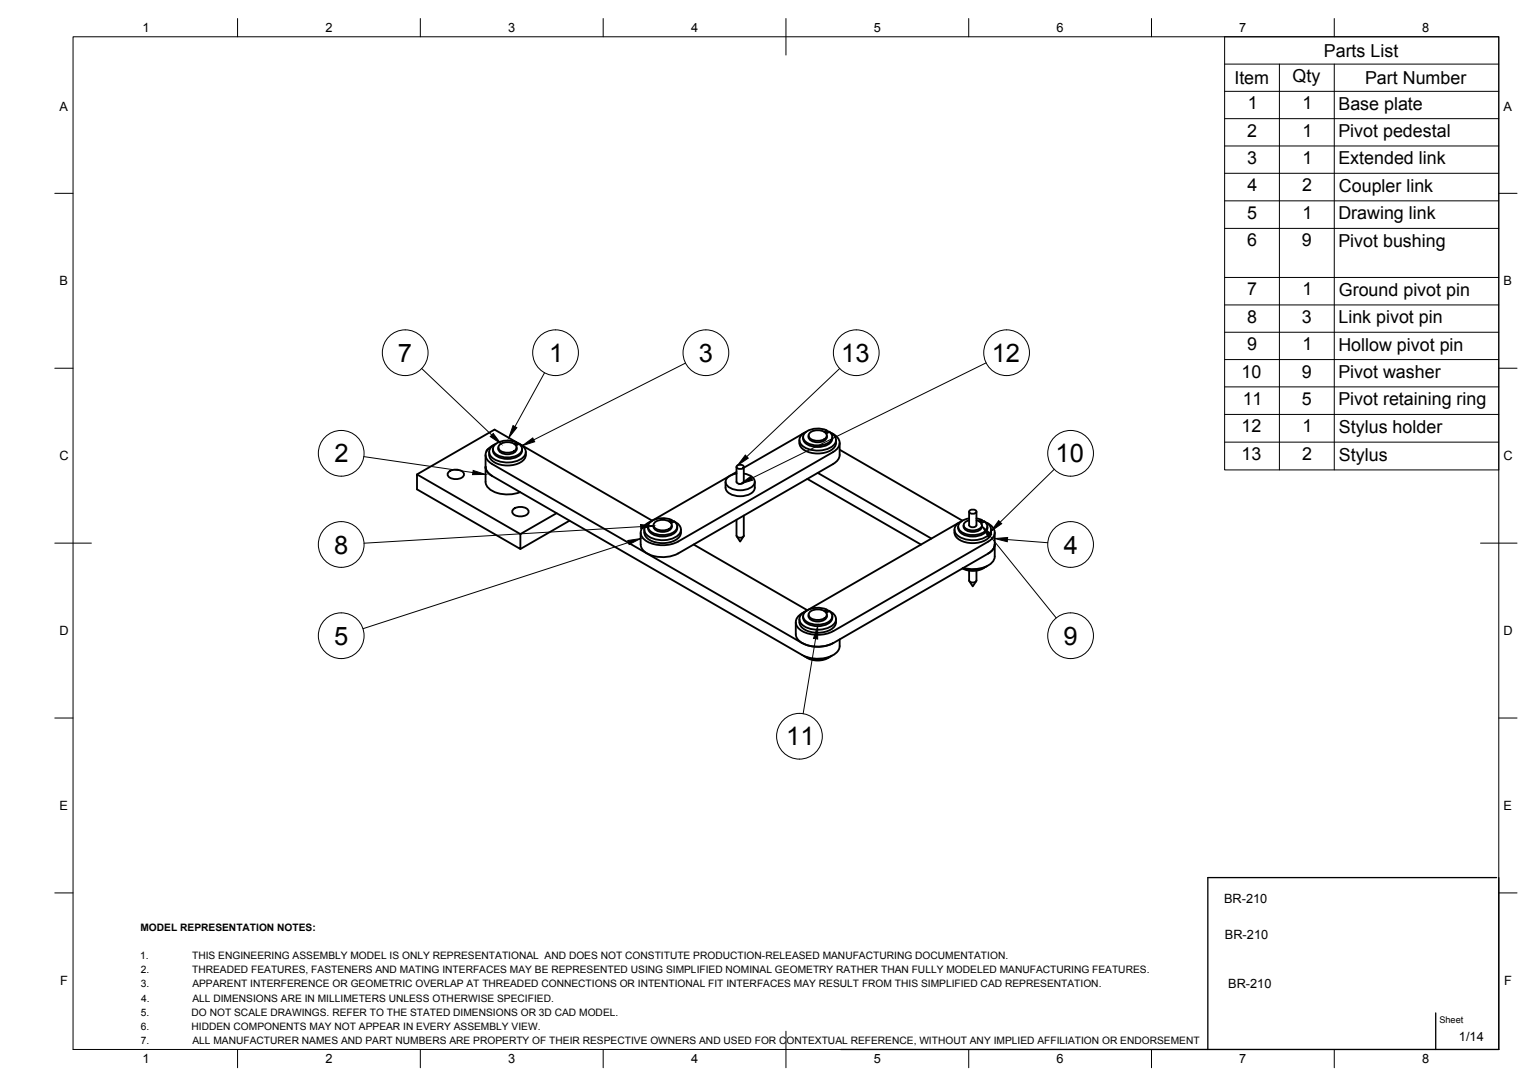
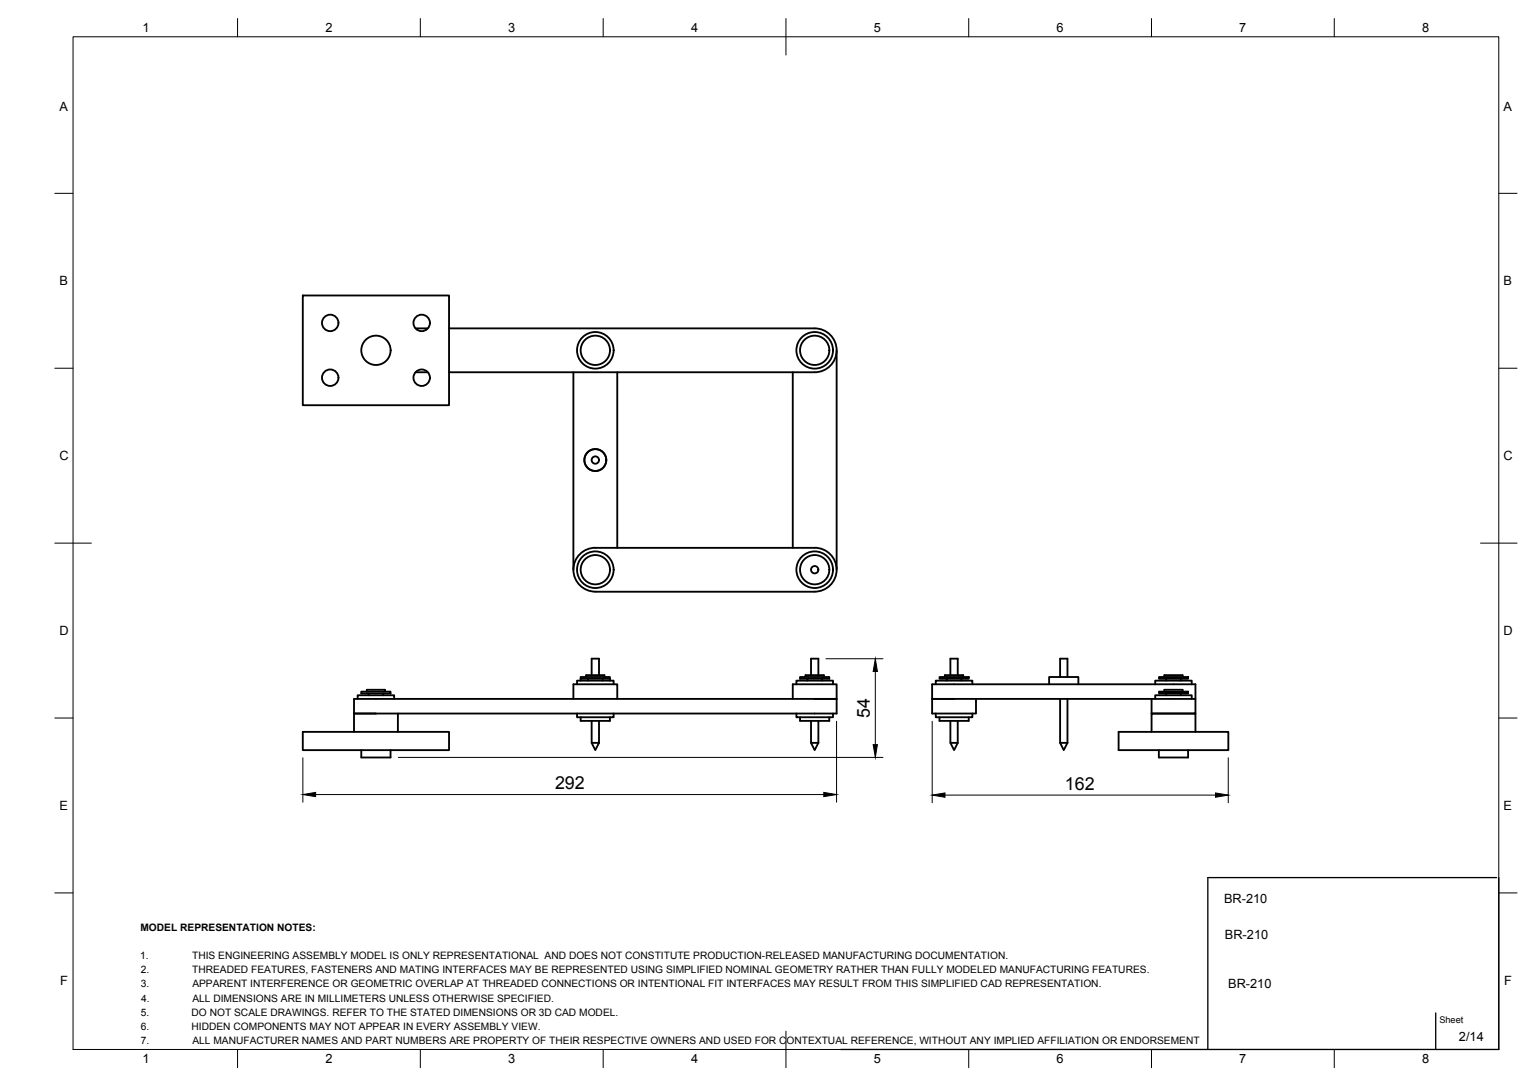
ISO-10303-21;
HEADER;
/* Generated by software containing ST-Developer
 * from STEP Tools, Inc. (www.steptools.com) 
 */

FILE_DESCRIPTION(
/* description */ ('Independent 1:2 reduction pantograph. 120 mm parallelogram sides; fix
ed fulcrum on the extension of a 240 mm link. Drawing point halfway al
ong its link, so its XY displacement is one half of the tracing point.
 Replaceable pivot bushes and retained pins. Calibration and productio
n accuracy unassigned.'),
/* implementation_level */ '2;1');

FILE_NAME(
/* name */ 'BR-210.step',
/* time_stamp */ '2026-11-07T22:11:57-08:00',
/* author */ (''),
/* organization */ (''),
/* preprocessor_version */ 'ST-DEVELOPER v20.2',
/* originating_system */ 'Autodesk Translation Framework v15.17.0.0',
/* authorisation */ '');

FILE_SCHEMA (('AUTOMOTIVE_DESIGN { 1 0 10303 214 3 1 1 }'));
ENDSEC;

DATA;
#10=MECHANICAL_DESIGN_GEOMETRIC_PRESENTATION_REPRESENTATION('',(#186,#187,
#188,#189,#190,#191,#192,#193,#194,#195,#196,#197,#198),#2926);
#11=ITEM_DEFINED_TRANSFORMATION($,$,#1699,#1892);
#12=ITEM_DEFINED_TRANSFORMATION($,$,#1721,#1893);
#13=ITEM_DEFINED_TRANSFORMATION($,$,#1730,#1894);
#14=ITEM_DEFINED_TRANSFORMATION($,$,#1822,#1895);
#15=ITEM_DEFINED_TRANSFORMATION($,$,#1750,#1896);
#16=ITEM_DEFINED_TRANSFORMATION($,$,#1839,#1897);
#17=ITEM_DEFINED_TRANSFORMATION($,$,#1770,#1898);
#18=ITEM_DEFINED_TRANSFORMATION($,$,#1848,#1899);
#19=ITEM_DEFINED_TRANSFORMATION($,$,#1788,#1900);
#20=ITEM_DEFINED_TRANSFORMATION($,$,#1866,#1901);
#21=ITEM_DEFINED_TRANSFORMATION($,$,#1875,#1902);
#22=ITEM_DEFINED_TRANSFORMATION($,$,#1809,#1903);
#23=ITEM_DEFINED_TRANSFORMATION($,$,#1886,#1904);
#24=ITEM_DEFINED_TRANSFORMATION($,$,#1822,#1905);
#25=ITEM_DEFINED_TRANSFORMATION($,$,#1839,#1906);
#26=ITEM_DEFINED_TRANSFORMATION($,$,#1839,#1907);
#27=ITEM_DEFINED_TRANSFORMATION($,$,#1839,#1908);
#28=ITEM_DEFINED_TRANSFORMATION($,$,#1839,#1909);
#29=ITEM_DEFINED_TRANSFORMATION($,$,#1839,#1910);
#30=ITEM_DEFINED_TRANSFORMATION($,$,#1839,#1911);
#31=ITEM_DEFINED_TRANSFORMATION($,$,#1839,#1912);
#32=ITEM_DEFINED_TRANSFORMATION($,$,#1839,#1913);
#33=ITEM_DEFINED_TRANSFORMATION($,$,#1866,#1914);
#34=ITEM_DEFINED_TRANSFORMATION($,$,#1866,#1915);
#35=ITEM_DEFINED_TRANSFORMATION($,$,#1875,#1916);
#36=ITEM_DEFINED_TRANSFORMATION($,$,#1848,#1917);
#37=ITEM_DEFINED_TRANSFORMATION($,$,#1866,#1918);
#38=ITEM_DEFINED_TRANSFORMATION($,$,#1866,#1919);
#39=ITEM_DEFINED_TRANSFORMATION($,$,#1875,#1920);
#40=ITEM_DEFINED_TRANSFORMATION($,$,#1848,#1921);
#41=ITEM_DEFINED_TRANSFORMATION($,$,#1866,#1922);
#42=ITEM_DEFINED_TRANSFORMATION($,$,#1866,#1923);
#43=ITEM_DEFINED_TRANSFORMATION($,$,#1875,#1924);
#44=ITEM_DEFINED_TRANSFORMATION($,$,#1866,#1925);
#45=ITEM_DEFINED_TRANSFORMATION($,$,#1866,#1926);
#46=ITEM_DEFINED_TRANSFORMATION($,$,#1875,#1927);
#47=ITEM_DEFINED_TRANSFORMATION($,$,#1886,#1928);
#48=(
REPRESENTATION_RELATIONSHIP($,$,#2997,#2996)
REPRESENTATION_RELATIONSHIP_WITH_TRANSFORMATION(#11)
SHAPE_REPRESENTATION_RELATIONSHIP()
);
#49=(
REPRESENTATION_RELATIONSHIP($,$,#2998,#2996)
REPRESENTATION_RELATIONSHIP_WITH_TRANSFORMATION(#12)
SHAPE_REPRESENTATION_RELATIONSHIP()
);
#50=(
REPRESENTATION_RELATIONSHIP($,$,#2999,#2996)
REPRESENTATION_RELATIONSHIP_WITH_TRANSFORMATION(#13)
SHAPE_REPRESENTATION_RELATIONSHIP()
);
#51=(
REPRESENTATION_RELATIONSHIP($,$,#3004,#2996)
REPRESENTATION_RELATIONSHIP_WITH_TRANSFORMATION(#14)
SHAPE_REPRESENTATION_RELATIONSHIP()
);
#52=(
REPRESENTATION_RELATIONSHIP($,$,#3000,#2996)
REPRESENTATION_RELATIONSHIP_WITH_TRANSFORMATION(#15)
SHAPE_REPRESENTATION_RELATIONSHIP()
);
#53=(
REPRESENTATION_RELATIONSHIP($,$,#3005,#2996)
REPRESENTATION_RELATIONSHIP_WITH_TRANSFORMATION(#16)
SHAPE_REPRESENTATION_RELATIONSHIP()
);
#54=(
REPRESENTATION_RELATIONSHIP($,$,#3001,#2996)
REPRESENTATION_RELATIONSHIP_WITH_TRANSFORMATION(#17)
SHAPE_REPRESENTATION_RELATIONSHIP()
);
#55=(
REPRESENTATION_RELATIONSHIP($,$,#3006,#2996)
REPRESENTATION_RELATIONSHIP_WITH_TRANSFORMATION(#18)
SHAPE_REPRESENTATION_RELATIONSHIP()
);
#56=(
REPRESENTATION_RELATIONSHIP($,$,#3002,#2996)
REPRESENTATION_RELATIONSHIP_WITH_TRANSFORMATION(#19)
SHAPE_REPRESENTATION_RELATIONSHIP()
);
#57=(
REPRESENTATION_RELATIONSHIP($,$,#3007,#2996)
REPRESENTATION_RELATIONSHIP_WITH_TRANSFORMATION(#20)
SHAPE_REPRESENTATION_RELATIONSHIP()
);
#58=(
REPRESENTATION_RELATIONSHIP($,$,#3008,#2996)
REPRESENTATION_RELATIONSHIP_WITH_TRANSFORMATION(#21)
SHAPE_REPRESENTATION_RELATIONSHIP()
);
#59=(
REPRESENTATION_RELATIONSHIP($,$,#3003,#2996)
REPRESENTATION_RELATIONSHIP_WITH_TRANSFORMATION(#22)
SHAPE_REPRESENTATION_RELATIONSHIP()
);
#60=(
REPRESENTATION_RELATIONSHIP($,$,#3009,#2996)
REPRESENTATION_RELATIONSHIP_WITH_TRANSFORMATION(#23)
SHAPE_REPRESENTATION_RELATIONSHIP()
);
#61=(
REPRESENTATION_RELATIONSHIP($,$,#3004,#2996)
REPRESENTATION_RELATIONSHIP_WITH_TRANSFORMATION(#24)
SHAPE_REPRESENTATION_RELATIONSHIP()
);
#62=(
REPRESENTATION_RELATIONSHIP($,$,#3005,#2996)
REPRESENTATION_RELATIONSHIP_WITH_TRANSFORMATION(#25)
SHAPE_REPRESENTATION_RELATIONSHIP()
);
#63=(
REPRESENTATION_RELATIONSHIP($,$,#3005,#2996)
REPRESENTATION_RELATIONSHIP_WITH_TRANSFORMATION(#26)
SHAPE_REPRESENTATION_RELATIONSHIP()
);
#64=(
REPRESENTATION_RELATIONSHIP($,$,#3005,#2996)
REPRESENTATION_RELATIONSHIP_WITH_TRANSFORMATION(#27)
SHAPE_REPRESENTATION_RELATIONSHIP()
);
#65=(
REPRESENTATION_RELATIONSHIP($,$,#3005,#2996)
REPRESENTATION_RELATIONSHIP_WITH_TRANSFORMATION(#28)
SHAPE_REPRESENTATION_RELATIONSHIP()
);
#66=(
REPRESENTATION_RELATIONSHIP($,$,#3005,#2996)
REPRESENTATION_RELATIONSHIP_WITH_TRANSFORMATION(#29)
SHAPE_REPRESENTATION_RELATIONSHIP()
);
#67=(
REPRESENTATION_RELATIONSHIP($,$,#3005,#2996)
REPRESENTATION_RELATIONSHIP_WITH_TRANSFORMATION(#30)
SHAPE_REPRESENTATION_RELATIONSHIP()
);
#68=(
REPRESENTATION_RELATIONSHIP($,$,#3005,#2996)
REPRESENTATION_RELATIONSHIP_WITH_TRANSFORMATION(#31)
SHAPE_REPRESENTATION_RELATIONSHIP()
);
#69=(
REPRESENTATION_RELATIONSHIP($,$,#3005,#2996)
REPRESENTATION_RELATIONSHIP_WITH_TRANSFORMATION(#32)
SHAPE_REPRESENTATION_RELATIONSHIP()
);
#70=(
REPRESENTATION_RELATIONSHIP($,$,#3007,#2996)
REPRESENTATION_RELATIONSHIP_WITH_TRANSFORMATION(#33)
SHAPE_REPRESENTATION_RELATIONSHIP()
);
#71=(
REPRESENTATION_RELATIONSHIP($,$,#3007,#2996)
REPRESENTATION_RELATIONSHIP_WITH_TRANSFORMATION(#34)
SHAPE_REPRESENTATION_RELATIONSHIP()
);
#72=(
REPRESENTATION_RELATIONSHIP($,$,#3008,#2996)
REPRESENTATION_RELATIONSHIP_WITH_TRANSFORMATION(#35)
SHAPE_REPRESENTATION_RELATIONSHIP()
);
#73=(
REPRESENTATION_RELATIONSHIP($,$,#3006,#2996)
REPRESENTATION_RELATIONSHIP_WITH_TRANSFORMATION(#36)
SHAPE_REPRESENTATION_RELATIONSHIP()
);
#74=(
REPRESENTATION_RELATIONSHIP($,$,#3007,#2996)
REPRESENTATION_RELATIONSHIP_WITH_TRANSFORMATION(#37)
SHAPE_REPRESENTATION_RELATIONSHIP()
);
#75=(
REPRESENTATION_RELATIONSHIP($,$,#3007,#2996)
REPRESENTATION_RELATIONSHIP_WITH_TRANSFORMATION(#38)
SHAPE_REPRESENTATION_RELATIONSHIP()
);
#76=(
REPRESENTATION_RELATIONSHIP($,$,#3008,#2996)
REPRESENTATION_RELATIONSHIP_WITH_TRANSFORMATION(#39)
SHAPE_REPRESENTATION_RELATIONSHIP()
);
#77=(
REPRESENTATION_RELATIONSHIP($,$,#3006,#2996)
REPRESENTATION_RELATIONSHIP_WITH_TRANSFORMATION(#40)
SHAPE_REPRESENTATION_RELATIONSHIP()
);
#78=(
REPRESENTATION_RELATIONSHIP($,$,#3007,#2996)
REPRESENTATION_RELATIONSHIP_WITH_TRANSFORMATION(#41)
SHAPE_REPRESENTATION_RELATIONSHIP()
);
#79=(
REPRESENTATION_RELATIONSHIP($,$,#3007,#2996)
REPRESENTATION_RELATIONSHIP_WITH_TRANSFORMATION(#42)
SHAPE_REPRESENTATION_RELATIONSHIP()
);
#80=(
REPRESENTATION_RELATIONSHIP($,$,#3008,#2996)
REPRESENTATION_RELATIONSHIP_WITH_TRANSFORMATION(#43)
SHAPE_REPRESENTATION_RELATIONSHIP()
);
#81=(
REPRESENTATION_RELATIONSHIP($,$,#3007,#2996)
REPRESENTATION_RELATIONSHIP_WITH_TRANSFORMATION(#44)
SHAPE_REPRESENTATION_RELATIONSHIP()
);
#82=(
REPRESENTATION_RELATIONSHIP($,$,#3007,#2996)
REPRESENTATION_RELATIONSHIP_WITH_TRANSFORMATION(#45)
SHAPE_REPRESENTATION_RELATIONSHIP()
);
#83=(
REPRESENTATION_RELATIONSHIP($,$,#3008,#2996)
REPRESENTATION_RELATIONSHIP_WITH_TRANSFORMATION(#46)
SHAPE_REPRESENTATION_RELATIONSHIP()
);
#84=(
REPRESENTATION_RELATIONSHIP($,$,#3009,#2996)
REPRESENTATION_RELATIONSHIP_WITH_TRANSFORMATION(#47)
SHAPE_REPRESENTATION_RELATIONSHIP()
);
#85=CONTEXT_DEPENDENT_SHAPE_REPRESENTATION(#48,#2959);
#86=CONTEXT_DEPENDENT_SHAPE_REPRESENTATION(#49,#2960);
#87=CONTEXT_DEPENDENT_SHAPE_REPRESENTATION(#50,#2961);
#88=CONTEXT_DEPENDENT_SHAPE_REPRESENTATION(#51,#2962);
#89=CONTEXT_DEPENDENT_SHAPE_REPRESENTATION(#52,#2963);
#90=CONTEXT_DEPENDENT_SHAPE_REPRESENTATION(#53,#2964);
#91=CONTEXT_DEPENDENT_SHAPE_REPRESENTATION(#54,#2965);
#92=CONTEXT_DEPENDENT_SHAPE_REPRESENTATION(#55,#2966);
#93=CONTEXT_DEPENDENT_SHAPE_REPRESENTATION(#56,#2967);
#94=CONTEXT_DEPENDENT_SHAPE_REPRESENTATION(#57,#2968);
#95=CONTEXT_DEPENDENT_SHAPE_REPRESENTATION(#58,#2969);
#96=CONTEXT_DEPENDENT_SHAPE_REPRESENTATION(#59,#2970);
#97=CONTEXT_DEPENDENT_SHAPE_REPRESENTATION(#60,#2971);
#98=CONTEXT_DEPENDENT_SHAPE_REPRESENTATION(#61,#2972);
#99=CONTEXT_DEPENDENT_SHAPE_REPRESENTATION(#62,#2973);
#100=CONTEXT_DEPENDENT_SHAPE_REPRESENTATION(#63,#2974);
#101=CONTEXT_DEPENDENT_SHAPE_REPRESENTATION(#64,#2975);
#102=CONTEXT_DEPENDENT_SHAPE_REPRESENTATION(#65,#2976);
#103=CONTEXT_DEPENDENT_SHAPE_REPRESENTATION(#66,#2977);
#104=CONTEXT_DEPENDENT_SHAPE_REPRESENTATION(#67,#2978);
#105=CONTEXT_DEPENDENT_SHAPE_REPRESENTATION(#68,#2979);
#106=CONTEXT_DEPENDENT_SHAPE_REPRESENTATION(#69,#2980);
#107=CONTEXT_DEPENDENT_SHAPE_REPRESENTATION(#70,#2981);
#108=CONTEXT_DEPENDENT_SHAPE_REPRESENTATION(#71,#2982);
#109=CONTEXT_DEPENDENT_SHAPE_REPRESENTATION(#72,#2983);
#110=CONTEXT_DEPENDENT_SHAPE_REPRESENTATION(#73,#2984);
#111=CONTEXT_DEPENDENT_SHAPE_REPRESENTATION(#74,#2985);
#112=CONTEXT_DEPENDENT_SHAPE_REPRESENTATION(#75,#2986);
#113=CONTEXT_DEPENDENT_SHAPE_REPRESENTATION(#76,#2987);
#114=CONTEXT_DEPENDENT_SHAPE_REPRESENTATION(#77,#2988);
#115=CONTEXT_DEPENDENT_SHAPE_REPRESENTATION(#78,#2989);
#116=CONTEXT_DEPENDENT_SHAPE_REPRESENTATION(#79,#2990);
#117=CONTEXT_DEPENDENT_SHAPE_REPRESENTATION(#80,#2991);
#118=CONTEXT_DEPENDENT_SHAPE_REPRESENTATION(#81,#2992);
#119=CONTEXT_DEPENDENT_SHAPE_REPRESENTATION(#82,#2993);
#120=CONTEXT_DEPENDENT_SHAPE_REPRESENTATION(#83,#2994);
#121=CONTEXT_DEPENDENT_SHAPE_REPRESENTATION(#84,#2995);
#122=NEXT_ASSEMBLY_USAGE_OCCURRENCE('Base plate:1','Base plate:1',
'Base plate:1',#3011,#3012,'Base plate:1');
#123=NEXT_ASSEMBLY_USAGE_OCCURRENCE('Pivot pedestal:1',
'Pivot pedestal:1','Pivot pedestal:1',#3011,#3013,'Pivot pedestal:1');
#124=NEXT_ASSEMBLY_USAGE_OCCURRENCE('Extended link:1','Extended link:1',
'Extended link:1',#3011,#3014,'Extended link:1');
#125=NEXT_ASSEMBLY_USAGE_OCCURRENCE('Coupler link:1','Coupler link:1',
'Coupler link:1',#3011,#3019,'Coupler link:1');
#126=NEXT_ASSEMBLY_USAGE_OCCURRENCE('Drawing link:1','Drawing link:1',
'Drawing link:1',#3011,#3015,'Drawing link:1');
#127=NEXT_ASSEMBLY_USAGE_OCCURRENCE('Pivot bushing:1','Pivot bushing:1',
'Pivot bushing:1',#3011,#3020,'Pivot bushing:1');
#128=NEXT_ASSEMBLY_USAGE_OCCURRENCE('Ground pivot pin:1',
'Ground pivot pin:1','Ground pivot pin:1',#3011,#3016,
'Ground pivot pin:1');
#129=NEXT_ASSEMBLY_USAGE_OCCURRENCE('Link pivot pin:1',
'Link pivot pin:1','Link pivot pin:1',#3011,#3021,'Link pivot pin:1');
#130=NEXT_ASSEMBLY_USAGE_OCCURRENCE('Hollow pivot pin:1',
'Hollow pivot pin:1','Hollow pivot pin:1',#3011,#3017,
'Hollow pivot pin:1');
#131=NEXT_ASSEMBLY_USAGE_OCCURRENCE('Pivot washer:1','Pivot washer:1',
'Pivot washer:1',#3011,#3022,'Pivot washer:1');
#132=NEXT_ASSEMBLY_USAGE_OCCURRENCE('Pivot retaining ring:1',
'Pivot retaining ring:1','Pivot retaining ring:1',#3011,#3023,
'Pivot retaining ring:1');
#133=NEXT_ASSEMBLY_USAGE_OCCURRENCE('Stylus holder:1','Stylus holder:1',
'Stylus holder:1',#3011,#3018,'Stylus holder:1');
#134=NEXT_ASSEMBLY_USAGE_OCCURRENCE('Stylus:1','Stylus:1','Stylus:1',#3011,
#3024,'Stylus:1');
#135=NEXT_ASSEMBLY_USAGE_OCCURRENCE('Coupler link:2','Coupler link:2',
'Coupler link:2',#3011,#3019,'Coupler link:2');
#136=NEXT_ASSEMBLY_USAGE_OCCURRENCE('Pivot bushing:2','Pivot bushing:2',
'Pivot bushing:2',#3011,#3020,'Pivot bushing:2');
#137=NEXT_ASSEMBLY_USAGE_OCCURRENCE('Pivot bushing:3','Pivot bushing:3',
'Pivot bushing:3',#3011,#3020,'Pivot bushing:3');
#138=NEXT_ASSEMBLY_USAGE_OCCURRENCE('Pivot bushing:4','Pivot bushing:4',
'Pivot bushing:4',#3011,#3020,'Pivot bushing:4');
#139=NEXT_ASSEMBLY_USAGE_OCCURRENCE('Pivot bushing:5','Pivot bushing:5',
'Pivot bushing:5',#3011,#3020,'Pivot bushing:5');
#140=NEXT_ASSEMBLY_USAGE_OCCURRENCE('Pivot bushing:6','Pivot bushing:6',
'Pivot bushing:6',#3011,#3020,'Pivot bushing:6');
#141=NEXT_ASSEMBLY_USAGE_OCCURRENCE('Pivot bushing:7','Pivot bushing:7',
'Pivot bushing:7',#3011,#3020,'Pivot bushing:7');
#142=NEXT_ASSEMBLY_USAGE_OCCURRENCE('Pivot bushing:8','Pivot bushing:8',
'Pivot bushing:8',#3011,#3020,'Pivot bushing:8');
#143=NEXT_ASSEMBLY_USAGE_OCCURRENCE('Pivot bushing:9','Pivot bushing:9',
'Pivot bushing:9',#3011,#3020,'Pivot bushing:9');
#144=NEXT_ASSEMBLY_USAGE_OCCURRENCE('Pivot washer:2','Pivot washer:2',
'Pivot washer:2',#3011,#3022,'Pivot washer:2');
#145=NEXT_ASSEMBLY_USAGE_OCCURRENCE('Pivot washer:3','Pivot washer:3',
'Pivot washer:3',#3011,#3022,'Pivot washer:3');
#146=NEXT_ASSEMBLY_USAGE_OCCURRENCE('Pivot retaining ring:2',
'Pivot retaining ring:2','Pivot retaining ring:2',#3011,#3023,
'Pivot retaining ring:2');
#147=NEXT_ASSEMBLY_USAGE_OCCURRENCE('Link pivot pin:2',
'Link pivot pin:2','Link pivot pin:2',#3011,#3021,'Link pivot pin:2');
#148=NEXT_ASSEMBLY_USAGE_OCCURRENCE('Pivot washer:4','Pivot washer:4',
'Pivot washer:4',#3011,#3022,'Pivot washer:4');
#149=NEXT_ASSEMBLY_USAGE_OCCURRENCE('Pivot washer:5','Pivot washer:5',
'Pivot washer:5',#3011,#3022,'Pivot washer:5');
#150=NEXT_ASSEMBLY_USAGE_OCCURRENCE('Pivot retaining ring:3',
'Pivot retaining ring:3','Pivot retaining ring:3',#3011,#3023,
'Pivot retaining ring:3');
#151=NEXT_ASSEMBLY_USAGE_OCCURRENCE('Link pivot pin:3',
'Link pivot pin:3','Link pivot pin:3',#3011,#3021,'Link pivot pin:3');
#152=NEXT_ASSEMBLY_USAGE_OCCURRENCE('Pivot washer:6','Pivot washer:6',
'Pivot washer:6',#3011,#3022,'Pivot washer:6');
#153=NEXT_ASSEMBLY_USAGE_OCCURRENCE('Pivot washer:7','Pivot washer:7',
'Pivot washer:7',#3011,#3022,'Pivot washer:7');
#154=NEXT_ASSEMBLY_USAGE_OCCURRENCE('Pivot retaining ring:4',
'Pivot retaining ring:4','Pivot retaining ring:4',#3011,#3023,
'Pivot retaining ring:4');
#155=NEXT_ASSEMBLY_USAGE_OCCURRENCE('Pivot washer:8','Pivot washer:8',
'Pivot washer:8',#3011,#3022,'Pivot washer:8');
#156=NEXT_ASSEMBLY_USAGE_OCCURRENCE('Pivot washer:9','Pivot washer:9',
'Pivot washer:9',#3011,#3022,'Pivot washer:9');
#157=NEXT_ASSEMBLY_USAGE_OCCURRENCE('Pivot retaining ring:5',
'Pivot retaining ring:5','Pivot retaining ring:5',#3011,#3023,
'Pivot retaining ring:5');
#158=NEXT_ASSEMBLY_USAGE_OCCURRENCE('Stylus:2','Stylus:2','Stylus:2',#3011,
#3024,'Stylus:2');
#159=CONICAL_SURFACE('',#1891,1.,0.463647609000806);
#160=SHAPE_REPRESENTATION_RELATIONSHIP('SRR','None',#2997,#173);
#161=SHAPE_REPRESENTATION_RELATIONSHIP('SRR','None',#2998,#174);
#162=SHAPE_REPRESENTATION_RELATIONSHIP('SRR','None',#2999,#175);
#163=SHAPE_REPRESENTATION_RELATIONSHIP('SRR','None',#3000,#176);
#164=SHAPE_REPRESENTATION_RELATIONSHIP('SRR','None',#3001,#177);
#165=SHAPE_REPRESENTATION_RELATIONSHIP('SRR','None',#3002,#178);
#166=SHAPE_REPRESENTATION_RELATIONSHIP('SRR','None',#3003,#179);
#167=SHAPE_REPRESENTATION_RELATIONSHIP('SRR','None',#3004,#180);
#168=SHAPE_REPRESENTATION_RELATIONSHIP('SRR','None',#3005,#181);
#169=SHAPE_REPRESENTATION_RELATIONSHIP('SRR','None',#3006,#182);
#170=SHAPE_REPRESENTATION_RELATIONSHIP('SRR','None',#3007,#183);
#171=SHAPE_REPRESENTATION_RELATIONSHIP('SRR','None',#3008,#184);
#172=SHAPE_REPRESENTATION_RELATIONSHIP('SRR','None',#3009,#185);
#173=ADVANCED_BREP_SHAPE_REPRESENTATION('',(#199),#2913);
#174=ADVANCED_BREP_SHAPE_REPRESENTATION('',(#200),#2914);
#175=ADVANCED_BREP_SHAPE_REPRESENTATION('',(#201),#2915);
#176=ADVANCED_BREP_SHAPE_REPRESENTATION('',(#202),#2916);
#177=ADVANCED_BREP_SHAPE_REPRESENTATION('',(#203),#2917);
#178=ADVANCED_BREP_SHAPE_REPRESENTATION('',(#204),#2918);
#179=ADVANCED_BREP_SHAPE_REPRESENTATION('',(#205),#2919);
#180=ADVANCED_BREP_SHAPE_REPRESENTATION('',(#206),#2920);
#181=ADVANCED_BREP_SHAPE_REPRESENTATION('',(#207),#2921);
#182=ADVANCED_BREP_SHAPE_REPRESENTATION('',(#208),#2922);
#183=ADVANCED_BREP_SHAPE_REPRESENTATION('',(#209),#2923);
#184=ADVANCED_BREP_SHAPE_REPRESENTATION('',(#210),#2924);
#185=ADVANCED_BREP_SHAPE_REPRESENTATION('',(#211),#2925);
#186=STYLED_ITEM('',(#3071),#199);
#187=STYLED_ITEM('',(#3072),#200);
#188=STYLED_ITEM('',(#3073),#201);
#189=STYLED_ITEM('',(#3074),#202);
#190=STYLED_ITEM('',(#3075),#203);
#191=STYLED_ITEM('',(#3075),#204);
#192=STYLED_ITEM('',(#3076),#205);
#193=STYLED_ITEM('',(#3077),#206);
#194=STYLED_ITEM('',(#3078),#207);
#195=STYLED_ITEM('',(#3075),#208);
#196=STYLED_ITEM('',(#3079),#209);
#197=STYLED_ITEM('',(#3080),#210);
#198=STYLED_ITEM('',(#3081),#211);
#199=MANIFOLD_SOLID_BREP('Body1',#1541);
#200=MANIFOLD_SOLID_BREP('Body1',#1542);
#201=MANIFOLD_SOLID_BREP('Body1',#1543);
#202=MANIFOLD_SOLID_BREP('Body1',#1544);
#203=MANIFOLD_SOLID_BREP('Body1',#1545);
#204=MANIFOLD_SOLID_BREP('Body1',#1546);
#205=MANIFOLD_SOLID_BREP('Body1',#1547);
#206=MANIFOLD_SOLID_BREP('Body1',#1548);
#207=MANIFOLD_SOLID_BREP('Body1',#1549);
#208=MANIFOLD_SOLID_BREP('Body1',#1550);
#209=MANIFOLD_SOLID_BREP('Body1',#1551);
#210=MANIFOLD_SOLID_BREP('Body1',#1552);
#211=MANIFOLD_SOLID_BREP('Body1',#1553);
#212=FACE_BOUND('',#407,.T.);
#213=FACE_BOUND('',#408,.T.);
#214=FACE_BOUND('',#409,.T.);
#215=FACE_BOUND('',#410,.T.);
#216=FACE_BOUND('',#411,.T.);
#217=FACE_BOUND('',#413,.T.);
#218=FACE_BOUND('',#414,.T.);
#219=FACE_BOUND('',#415,.T.);
#220=FACE_BOUND('',#416,.T.);
#221=FACE_BOUND('',#417,.T.);
#222=FACE_BOUND('',#421,.T.);
#223=FACE_BOUND('',#423,.T.);
#224=FACE_BOUND('',#432,.T.);
#225=FACE_BOUND('',#433,.T.);
#226=FACE_BOUND('',#434,.T.);
#227=FACE_BOUND('',#436,.T.);
#228=FACE_BOUND('',#437,.T.);
#229=FACE_BOUND('',#438,.T.);
#230=FACE_BOUND('',#447,.T.);
#231=FACE_BOUND('',#448,.T.);
#232=FACE_BOUND('',#449,.T.);
#233=FACE_BOUND('',#451,.T.);
#234=FACE_BOUND('',#452,.T.);
#235=FACE_BOUND('',#453,.T.);
#236=FACE_BOUND('',#456,.T.);
#237=FACE_BOUND('',#458,.T.);
#238=FACE_BOUND('',#461,.T.);
#239=FACE_BOUND('',#468,.T.);
#240=FACE_BOUND('',#470,.T.);
#241=FACE_BOUND('',#473,.T.);
#242=FACE_BOUND('',#476,.T.);
#243=FACE_BOUND('',#480,.T.);
#244=FACE_BOUND('',#482,.T.);
#245=FACE_BOUND('',#485,.T.);
#246=FACE_BOUND('',#489,.T.);
#247=FACE_BOUND('',#497,.T.);
#248=FACE_BOUND('',#498,.T.);
#249=FACE_BOUND('',#500,.T.);
#250=FACE_BOUND('',#501,.T.);
#251=FACE_BOUND('',#505,.T.);
#252=FACE_BOUND('',#507,.T.);
#253=FACE_BOUND('',#510,.T.);
#254=FACE_BOUND('',#512,.T.);
#255=FACE_BOUND('',#515,.T.);
#256=FACE_BOUND('',#523,.T.);
#257=FACE_BOUND('',#525,.T.);
#258=PLANE('',#1715);
#259=PLANE('',#1716);
#260=PLANE('',#1717);
#261=PLANE('',#1718);
#262=PLANE('',#1719);
#263=PLANE('',#1720);
#264=PLANE('',#1728);
#265=PLANE('',#1729);
#266=PLANE('',#1740);
#267=PLANE('',#1744);
#268=PLANE('',#1748);
#269=PLANE('',#1749);
#270=PLANE('',#1760);
#271=PLANE('',#1764);
#272=PLANE('',#1768);
#273=PLANE('',#1769);
#274=PLANE('',#1774);
#275=PLANE('',#1776);
#276=PLANE('',#1780);
#277=PLANE('',#1785);
#278=PLANE('',#1787);
#279=PLANE('',#1792);
#280=PLANE('',#1794);
#281=PLANE('',#1798);
#282=PLANE('',#1803);
#283=PLANE('',#1808);
#284=PLANE('',#1810);
#285=PLANE('',#1815);
#286=PLANE('',#1821);
#287=PLANE('',#1829);
#288=PLANE('',#1833);
#289=PLANE('',#1837);
#290=PLANE('',#1838);
#291=PLANE('',#1846);
#292=PLANE('',#1847);
#293=PLANE('',#1852);
#294=PLANE('',#1854);
#295=PLANE('',#1858);
#296=PLANE('',#1863);
#297=PLANE('',#1865);
#298=PLANE('',#1873);
#299=PLANE('',#1874);
#300=PLANE('',#1876);
#301=PLANE('',#1877);
#302=PLANE('',#1878);
#303=PLANE('',#1885);
#304=PLANE('',#1890);
#305=FACE_OUTER_BOUND('',#397,.T.);
#306=FACE_OUTER_BOUND('',#398,.T.);
#307=FACE_OUTER_BOUND('',#399,.T.);
#308=FACE_OUTER_BOUND('',#400,.T.);
#309=FACE_OUTER_BOUND('',#401,.T.);
#310=FACE_OUTER_BOUND('',#402,.T.);
#311=FACE_OUTER_BOUND('',#403,.T.);
#312=FACE_OUTER_BOUND('',#404,.T.);
#313=FACE_OUTER_BOUND('',#405,.T.);
#314=FACE_OUTER_BOUND('',#406,.T.);
#315=FACE_OUTER_BOUND('',#412,.T.);
#316=FACE_OUTER_BOUND('',#418,.T.);
#317=FACE_OUTER_BOUND('',#419,.T.);
#318=FACE_OUTER_BOUND('',#420,.T.);
#319=FACE_OUTER_BOUND('',#422,.T.);
#320=FACE_OUTER_BOUND('',#424,.T.);
#321=FACE_OUTER_BOUND('',#425,.T.);
#322=FACE_OUTER_BOUND('',#426,.T.);
#323=FACE_OUTER_BOUND('',#427,.T.);
#324=FACE_OUTER_BOUND('',#428,.T.);
#325=FACE_OUTER_BOUND('',#429,.T.);
#326=FACE_OUTER_BOUND('',#430,.T.);
#327=FACE_OUTER_BOUND('',#431,.T.);
#328=FACE_OUTER_BOUND('',#435,.T.);
#329=FACE_OUTER_BOUND('',#439,.T.);
#330=FACE_OUTER_BOUND('',#440,.T.);
#331=FACE_OUTER_BOUND('',#441,.T.);
#332=FACE_OUTER_BOUND('',#442,.T.);
#333=FACE_OUTER_BOUND('',#443,.T.);
#334=FACE_OUTER_BOUND('',#444,.T.);
#335=FACE_OUTER_BOUND('',#445,.T.);
#336=FACE_OUTER_BOUND('',#446,.T.);
#337=FACE_OUTER_BOUND('',#450,.T.);
#338=FACE_OUTER_BOUND('',#454,.T.);
#339=FACE_OUTER_BOUND('',#455,.T.);
#340=FACE_OUTER_BOUND('',#457,.T.);
#341=FACE_OUTER_BOUND('',#459,.T.);
#342=FACE_OUTER_BOUND('',#460,.T.);
#343=FACE_OUTER_BOUND('',#462,.T.);
#344=FACE_OUTER_BOUND('',#463,.T.);
#345=FACE_OUTER_BOUND('',#464,.T.);
#346=FACE_OUTER_BOUND('',#465,.T.);
#347=FACE_OUTER_BOUND('',#466,.T.);
#348=FACE_OUTER_BOUND('',#467,.T.);
#349=FACE_OUTER_BOUND('',#469,.T.);
#350=FACE_OUTER_BOUND('',#471,.T.);
#351=FACE_OUTER_BOUND('',#472,.T.);
#352=FACE_OUTER_BOUND('',#474,.T.);
#353=FACE_OUTER_BOUND('',#475,.T.);
#354=FACE_OUTER_BOUND('',#477,.T.);
#355=FACE_OUTER_BOUND('',#478,.T.);
#356=FACE_OUTER_BOUND('',#479,.T.);
#357=FACE_OUTER_BOUND('',#481,.T.);
#358=FACE_OUTER_BOUND('',#483,.T.);
#359=FACE_OUTER_BOUND('',#484,.T.);
#360=FACE_OUTER_BOUND('',#486,.T.);
#361=FACE_OUTER_BOUND('',#487,.T.);
#362=FACE_OUTER_BOUND('',#488,.T.);
#363=FACE_OUTER_BOUND('',#490,.T.);
#364=FACE_OUTER_BOUND('',#491,.T.);
#365=FACE_OUTER_BOUND('',#492,.T.);
#366=FACE_OUTER_BOUND('',#493,.T.);
#367=FACE_OUTER_BOUND('',#494,.T.);
#368=FACE_OUTER_BOUND('',#495,.T.);
#369=FACE_OUTER_BOUND('',#496,.T.);
#370=FACE_OUTER_BOUND('',#499,.T.);
#371=FACE_OUTER_BOUND('',#502,.T.);
#372=FACE_OUTER_BOUND('',#503,.T.);
#373=FACE_OUTER_BOUND('',#504,.T.);
#374=FACE_OUTER_BOUND('',#506,.T.);
#375=FACE_OUTER_BOUND('',#508,.T.);
#376=FACE_OUTER_BOUND('',#509,.T.);
#377=FACE_OUTER_BOUND('',#511,.T.);
#378=FACE_OUTER_BOUND('',#513,.T.);
#379=FACE_OUTER_BOUND('',#514,.T.);
#380=FACE_OUTER_BOUND('',#516,.T.);
#381=FACE_OUTER_BOUND('',#517,.T.);
#382=FACE_OUTER_BOUND('',#518,.T.);
#383=FACE_OUTER_BOUND('',#519,.T.);
#384=FACE_OUTER_BOUND('',#520,.T.);
#385=FACE_OUTER_BOUND('',#521,.T.);
#386=FACE_OUTER_BOUND('',#522,.T.);
#387=FACE_OUTER_BOUND('',#524,.T.);
#388=FACE_OUTER_BOUND('',#526,.T.);
#389=FACE_OUTER_BOUND('',#527,.T.);
#390=FACE_OUTER_BOUND('',#528,.T.);
#391=FACE_OUTER_BOUND('',#529,.T.);
#392=FACE_OUTER_BOUND('',#530,.T.);
#393=FACE_OUTER_BOUND('',#531,.T.);
#394=FACE_OUTER_BOUND('',#532,.T.);
#395=FACE_OUTER_BOUND('',#533,.T.);
#396=FACE_OUTER_BOUND('',#534,.T.);
#397=EDGE_LOOP('',(#1067,#1068,#1069,#1070));
#398=EDGE_LOOP('',(#1071,#1072,#1073,#1074));
#399=EDGE_LOOP('',(#1075,#1076,#1077,#1078));
#400=EDGE_LOOP('',(#1079,#1080,#1081,#1082));
#401=EDGE_LOOP('',(#1083,#1084,#1085,#1086));
#402=EDGE_LOOP('',(#1087,#1088,#1089,#1090));
#403=EDGE_LOOP('',(#1091,#1092,#1093,#1094));
#404=EDGE_LOOP('',(#1095,#1096,#1097,#1098));
#405=EDGE_LOOP('',(#1099,#1100,#1101,#1102));
#406=EDGE_LOOP('',(#1103,#1104,#1105,#1106));
#407=EDGE_LOOP('',(#1107));
#408=EDGE_LOOP('',(#1108));
#409=EDGE_LOOP('',(#1109));
#410=EDGE_LOOP('',(#1110));
#411=EDGE_LOOP('',(#1111));
#412=EDGE_LOOP('',(#1112,#1113,#1114,#1115));
#413=EDGE_LOOP('',(#1116));
#414=EDGE_LOOP('',(#1117));
#415=EDGE_LOOP('',(#1118));
#416=EDGE_LOOP('',(#1119));
#417=EDGE_LOOP('',(#1120));
#418=EDGE_LOOP('',(#1121,#1122,#1123,#1124));
#419=EDGE_LOOP('',(#1125,#1126,#1127,#1128));
#420=EDGE_LOOP('',(#1129));
#421=EDGE_LOOP('',(#1130));
#422=EDGE_LOOP('',(#1131));
#423=EDGE_LOOP('',(#1132));
#424=EDGE_LOOP('',(#1133,#1134,#1135,#1136));
#425=EDGE_LOOP('',(#1137,#1138,#1139,#1140));
#426=EDGE_LOOP('',(#1141,#1142,#1143,#1144));
#427=EDGE_LOOP('',(#1145,#1146,#1147,#1148));
#428=EDGE_LOOP('',(#1149,#1150,#1151,#1152));
#429=EDGE_LOOP('',(#1153,#1154,#1155,#1156));
#430=EDGE_LOOP('',(#1157,#1158,#1159,#1160));
#431=EDGE_LOOP('',(#1161,#1162,#1163,#1164));
#432=EDGE_LOOP('',(#1165));
#433=EDGE_LOOP('',(#1166));
#434=EDGE_LOOP('',(#1167));
#435=EDGE_LOOP('',(#1168,#1169,#1170,#1171));
#436=EDGE_LOOP('',(#1172));
#437=EDGE_LOOP('',(#1173));
#438=EDGE_LOOP('',(#1174));
#439=EDGE_LOOP('',(#1175,#1176,#1177,#1178));
#440=EDGE_LOOP('',(#1179,#1180,#1181,#1182));
#441=EDGE_LOOP('',(#1183,#1184,#1185,#1186));
#442=EDGE_LOOP('',(#1187,#1188,#1189,#1190));
#443=EDGE_LOOP('',(#1191,#1192,#1193,#1194));
#444=EDGE_LOOP('',(#1195,#1196,#1197,#1198));
#445=EDGE_LOOP('',(#1199,#1200,#1201,#1202));
#446=EDGE_LOOP('',(#1203,#1204,#1205,#1206));
#447=EDGE_LOOP('',(#1207));
#448=EDGE_LOOP('',(#1208));
#449=EDGE_LOOP('',(#1209));
#450=EDGE_LOOP('',(#1210,#1211,#1212,#1213));
#451=EDGE_LOOP('',(#1214));
#452=EDGE_LOOP('',(#1215));
#453=EDGE_LOOP('',(#1216));
#454=EDGE_LOOP('',(#1217,#1218,#1219,#1220));
#455=EDGE_LOOP('',(#1221));
#456=EDGE_LOOP('',(#1222));
#457=EDGE_LOOP('',(#1223));
#458=EDGE_LOOP('',(#1224));
#459=EDGE_LOOP('',(#1225,#1226,#1227,#1228));
#460=EDGE_LOOP('',(#1229));
#461=EDGE_LOOP('',(#1230));
#462=EDGE_LOOP('',(#1231,#1232,#1233,#1234));
#463=EDGE_LOOP('',(#1235));
#464=EDGE_LOOP('',(#1236,#1237,#1238,#1239));
#465=EDGE_LOOP('',(#1240));
#466=EDGE_LOOP('',(#1241,#1242,#1243,#1244));
#467=EDGE_LOOP('',(#1245));
#468=EDGE_LOOP('',(#1246));
#469=EDGE_LOOP('',(#1247));
#470=EDGE_LOOP('',(#1248));
#471=EDGE_LOOP('',(#1249,#1250,#1251,#1252));
#472=EDGE_LOOP('',(#1253));
#473=EDGE_LOOP('',(#1254));
#474=EDGE_LOOP('',(#1255,#1256,#1257,#1258));
#475=EDGE_LOOP('',(#1259));
#476=EDGE_LOOP('',(#1260));
#477=EDGE_LOOP('',(#1261,#1262,#1263,#1264));
#478=EDGE_LOOP('',(#1265,#1266,#1267,#1268));
#479=EDGE_LOOP('',(#1269));
#480=EDGE_LOOP('',(#1270));
#481=EDGE_LOOP('',(#1271));
#482=EDGE_LOOP('',(#1272));
#483=EDGE_LOOP('',(#1273,#1274,#1275,#1276));
#484=EDGE_LOOP('',(#1277));
#485=EDGE_LOOP('',(#1278));
#486=EDGE_LOOP('',(#1279,#1280,#1281,#1282));
#487=EDGE_LOOP('',(#1283,#1284,#1285,#1286));
#488=EDGE_LOOP('',(#1287));
#489=EDGE_LOOP('',(#1288));
#490=EDGE_LOOP('',(#1289,#1290,#1291,#1292));
#491=EDGE_LOOP('',(#1293,#1294,#1295,#1296));
#492=EDGE_LOOP('',(#1297,#1298,#1299,#1300));
#493=EDGE_LOOP('',(#1301,#1302,#1303,#1304));
#494=EDGE_LOOP('',(#1305,#1306,#1307,#1308));
#495=EDGE_LOOP('',(#1309,#1310,#1311,#1312));
#496=EDGE_LOOP('',(#1313,#1314,#1315,#1316));
#497=EDGE_LOOP('',(#1317));
#498=EDGE_LOOP('',(#1318));
#499=EDGE_LOOP('',(#1319,#1320,#1321,#1322));
#500=EDGE_LOOP('',(#1323));
#501=EDGE_LOOP('',(#1324));
#502=EDGE_LOOP('',(#1325,#1326,#1327,#1328));
#503=EDGE_LOOP('',(#1329,#1330,#1331,#1332));
#504=EDGE_LOOP('',(#1333));
#505=EDGE_LOOP('',(#1334));
#506=EDGE_LOOP('',(#1335));
#507=EDGE_LOOP('',(#1336));
#508=EDGE_LOOP('',(#1337,#1338,#1339,#1340));
#509=EDGE_LOOP('',(#1341));
#510=EDGE_LOOP('',(#1342));
#511=EDGE_LOOP('',(#1343));
#512=EDGE_LOOP('',(#1344));
#513=EDGE_LOOP('',(#1345,#1346,#1347,#1348));
#514=EDGE_LOOP('',(#1349));
#515=EDGE_LOOP('',(#1350));
#516=EDGE_LOOP('',(#1351,#1352,#1353,#1354));
#517=EDGE_LOOP('',(#1355));
#518=EDGE_LOOP('',(#1356,#1357,#1358,#1359));
#519=EDGE_LOOP('',(#1360));
#520=EDGE_LOOP('',(#1361,#1362,#1363,#1364));
#521=EDGE_LOOP('',(#1365,#1366,#1367,#1368));
#522=EDGE_LOOP('',(#1369));
#523=EDGE_LOOP('',(#1370));
#524=EDGE_LOOP('',(#1371));
#525=EDGE_LOOP('',(#1372));
#526=EDGE_LOOP('',(#1373,#1374,#1375,#1376));
#527=EDGE_LOOP('',(#1377,#1378,#1379,#1380));
#528=EDGE_LOOP('',(#1381,#1382,#1383,#1384));
#529=EDGE_LOOP('',(#1385,#1386,#1387,#1388));
#530=EDGE_LOOP('',(#1389,#1390,#1391,#1392));
#531=EDGE_LOOP('',(#1393,#1394,#1395,#1396));
#532=EDGE_LOOP('',(#1397,#1398,#1399,#1400));
#533=EDGE_LOOP('',(#1401));
#534=EDGE_LOOP('',(#1402,#1403,#1404));
#535=LINE('',#2478,#616);
#536=LINE('',#2484,#617);
#537=LINE('',#2490,#618);
#538=LINE('',#2496,#619);
#539=LINE('',#2502,#620);
#540=LINE('',#2507,#621);
#541=LINE('',#2509,#622);
#542=LINE('',#2511,#623);
#543=LINE('',#2512,#624);
#544=LINE('',#2515,#625);
#545=LINE('',#2517,#626);
#546=LINE('',#2518,#627);
#547=LINE('',#2521,#628);
#548=LINE('',#2523,#629);
#549=LINE('',#2524,#630);
#550=LINE('',#2526,#631);
#551=LINE('',#2527,#632);
#552=LINE('',#2535,#633);
#553=LINE('',#2541,#634);
#554=LINE('',#2550,#635);
#555=LINE('',#2556,#636);
#556=LINE('',#2562,#637);
#557=LINE('',#2567,#638);
#558=LINE('',#2569,#639);
#559=LINE('',#2571,#640);
#560=LINE('',#2572,#641);
#561=LINE('',#2578,#642);
#562=LINE('',#2581,#643);
#563=LINE('',#2583,#644);
#564=LINE('',#2584,#645);
#565=LINE('',#2595,#646);
#566=LINE('',#2601,#647);
#567=LINE('',#2607,#648);
#568=LINE('',#2612,#649);
#569=LINE('',#2614,#650);
#570=LINE('',#2616,#651);
#571=LINE('',#2617,#652);
#572=LINE('',#2623,#653);
#573=LINE('',#2626,#654);
#574=LINE('',#2628,#655);
#575=LINE('',#2629,#656);
#576=LINE('',#2640,#657);
#577=LINE('',#2651,#658);
#578=LINE('',#2659,#659);
#579=LINE('',#2663,#660);
#580=LINE('',#2670,#661);
#581=LINE('',#2681,#662);
#582=LINE('',#2689,#663);
#583=LINE('',#2697,#664);
#584=LINE('',#2699,#665);
#585=LINE('',#2710,#666);
#586=LINE('',#2716,#667);
#587=LINE('',#2720,#668);
#588=LINE('',#2728,#669);
#589=LINE('',#2734,#670);
#590=LINE('',#2739,#671);
#591=LINE('',#2741,#672);
#592=LINE('',#2743,#673);
#593=LINE('',#2744,#674);
#594=LINE('',#2750,#675);
#595=LINE('',#2753,#676);
#596=LINE('',#2755,#677);
#597=LINE('',#2756,#678);
#598=LINE('',#2767,#679);
#599=LINE('',#2773,#680);
#600=LINE('',#2782,#681);
#601=LINE('',#2793,#682);
#602=LINE('',#2801,#683);
#603=LINE('',#2805,#684);
#604=LINE('',#2812,#685);
#605=LINE('',#2818,#686);
#606=LINE('',#2826,#687);
#607=LINE('',#2828,#688);
#608=LINE('',#2830,#689);
#609=LINE('',#2831,#690);
#610=LINE('',#2835,#691);
#611=LINE('',#2837,#692);
#612=LINE('',#2839,#693);
#613=LINE('',#2840,#694);
#614=LINE('',#2854,#695);
#615=LINE('',#2859,#696);
#616=VECTOR('',#1937,4.5);
#617=VECTOR('',#1944,4.5);
#618=VECTOR('',#1951,4.5);
#619=VECTOR('',#1958,4.5);
#620=VECTOR('',#1965,5.);
#621=VECTOR('',#1970,10.);
#622=VECTOR('',#1971,10.);
#623=VECTOR('',#1972,10.);
#624=VECTOR('',#1973,10.);
#625=VECTOR('',#1976,10.);
#626=VECTOR('',#1977,10.);
#627=VECTOR('',#1978,10.);
#628=VECTOR('',#1981,10.);
#629=VECTOR('',#1982,10.);
#630=VECTOR('',#1983,10.);
#631=VECTOR('',#1986,10.);
#632=VECTOR('',#1987,10.);
#633=VECTOR('',#1998,5.);
#634=VECTOR('',#2005,12.);
#635=VECTOR('',#2018,7.);
#636=VECTOR('',#2025,7.);
#637=VECTOR('',#2032,7.);
#638=VECTOR('',#2037,10.);
#639=VECTOR('',#2038,10.);
#640=VECTOR('',#2039,10.);
#641=VECTOR('',#2040,10.);
#642=VECTOR('',#2047,10.);
#643=VECTOR('',#2050,10.);
#644=VECTOR('',#2051,10.);
#645=VECTOR('',#2052,10.);
#646=VECTOR('',#2069,6.);
#647=VECTOR('',#2076,7.);
#648=VECTOR('',#2083,7.);
#649=VECTOR('',#2088,10.);
#650=VECTOR('',#2089,10.);
#651=VECTOR('',#2090,10.);
#652=VECTOR('',#2091,10.);
#653=VECTOR('',#2098,10.);
#654=VECTOR('',#2101,10.);
#655=VECTOR('',#2102,10.);
#656=VECTOR('',#2103,10.);
#657=VECTOR('',#2120,4.);
#658=VECTOR('',#2135,5.);
#659=VECTOR('',#2144,8.);
#660=VECTOR('',#2151,5.);
#661=VECTOR('',#2160,4.);
#662=VECTOR('',#2175,5.);
#663=VECTOR('',#2184,8.);
#664=VECTOR('',#2195,2.);
#665=VECTOR('',#2198,5.);
#666=VECTOR('',#2213,8.);
#667=VECTOR('',#2220,2.);
#668=VECTOR('',#2225,6.);
#669=VECTOR('',#2236,7.);
#670=VECTOR('',#2243,7.);
#671=VECTOR('',#2248,10.);
#672=VECTOR('',#2249,10.);
#673=VECTOR('',#2250,10.);
#674=VECTOR('',#2251,10.);
#675=VECTOR('',#2258,10.);
#676=VECTOR('',#2261,10.);
#677=VECTOR('',#2262,10.);
#678=VECTOR('',#2263,10.);
#679=VECTOR('',#2280,5.);
#680=VECTOR('',#2287,7.);
#681=VECTOR('',#2300,4.);
#682=VECTOR('',#2315,5.);
#683=VECTOR('',#2324,8.);
#684=VECTOR('',#2331,5.);
#685=VECTOR('',#2340,5.);
#686=VECTOR('',#2347,10.);
#687=VECTOR('',#2358,10.);
#688=VECTOR('',#2359,10.);
#689=VECTOR('',#2360,10.);
#690=VECTOR('',#2361,10.);
#691=VECTOR('',#2364,10.);
#692=VECTOR('',#2365,10.);
#693=VECTOR('',#2366,10.);
#694=VECTOR('',#2367,10.);
#695=VECTOR('',#2390,2.);
#696=VECTOR('',#2397,1.);
#697=CIRCLE('',#1701,4.5);
#698=CIRCLE('',#1702,4.5);
#699=CIRCLE('',#1704,4.5);
#700=CIRCLE('',#1705,4.5);
#701=CIRCLE('',#1707,4.5);
#702=CIRCLE('',#1708,4.5);
#703=CIRCLE('',#1710,4.5);
#704=CIRCLE('',#1711,4.5);
#705=CIRCLE('',#1713,5.);
#706=CIRCLE('',#1714,5.);
#707=CIRCLE('',#1723,5.);
#708=CIRCLE('',#1724,5.);
#709=CIRCLE('',#1726,12.);
#710=CIRCLE('',#1727,12.);
#711=CIRCLE('',#1732,7.);
#712=CIRCLE('',#1733,7.);
#713=CIRCLE('',#1735,7.);
#714=CIRCLE('',#1736,7.);
#715=CIRCLE('',#1738,7.);
#716=CIRCLE('',#1739,7.);
#717=CIRCLE('',#1742,12.);
#718=CIRCLE('',#1743,12.);
#719=CIRCLE('',#1746,12.);
#720=CIRCLE('',#1747,12.);
#721=CIRCLE('',#1752,6.);
#722=CIRCLE('',#1753,6.);
#723=CIRCLE('',#1755,7.);
#724=CIRCLE('',#1756,7.);
#725=CIRCLE('',#1758,7.);
#726=CIRCLE('',#1759,7.);
#727=CIRCLE('',#1762,12.);
#728=CIRCLE('',#1763,12.);
#729=CIRCLE('',#1766,12.);
#730=CIRCLE('',#1767,12.);
#731=CIRCLE('',#1772,4.);
#732=CIRCLE('',#1773,4.);
#733=CIRCLE('',#1775,5.);
#734=CIRCLE('',#1777,5.);
#735=CIRCLE('',#1779,5.);
#736=CIRCLE('',#1781,8.);
#737=CIRCLE('',#1782,5.);
#738=CIRCLE('',#1784,8.);
#739=CIRCLE('',#1790,4.);
#740=CIRCLE('',#1791,4.);
#741=CIRCLE('',#1793,5.);
#742=CIRCLE('',#1795,5.);
#743=CIRCLE('',#1797,5.);
#744=CIRCLE('',#1799,8.);
#745=CIRCLE('',#1800,5.);
#746=CIRCLE('',#1802,8.);
#747=CIRCLE('',#1804,2.);
#748=CIRCLE('',#1806,2.);
#749=CIRCLE('',#1811,8.);
#750=CIRCLE('',#1812,6.);
#751=CIRCLE('',#1814,8.);
#752=CIRCLE('',#1816,2.);
#753=CIRCLE('',#1818,2.);
#754=CIRCLE('',#1820,6.);
#755=CIRCLE('',#1824,7.);
#756=CIRCLE('',#1825,7.);
#757=CIRCLE('',#1827,7.);
#758=CIRCLE('',#1828,7.);
#759=CIRCLE('',#1831,12.);
#760=CIRCLE('',#1832,12.);
#761=CIRCLE('',#1835,12.);
#762=CIRCLE('',#1836,12.);
#763=CIRCLE('',#1841,5.);
#764=CIRCLE('',#1842,5.);
#765=CIRCLE('',#1844,7.);
#766=CIRCLE('',#1845,7.);
#767=CIRCLE('',#1850,4.);
#768=CIRCLE('',#1851,4.);
#769=CIRCLE('',#1853,5.);
#770=CIRCLE('',#1855,5.);
#771=CIRCLE('',#1857,5.);
#772=CIRCLE('',#1859,8.);
#773=CIRCLE('',#1860,5.);
#774=CIRCLE('',#1862,8.);
#775=CIRCLE('',#1868,5.);
#776=CIRCLE('',#1869,5.);
#777=CIRCLE('',#1871,10.);
#778=CIRCLE('',#1872,10.);
#779=CIRCLE('',#1879,8.);
#780=CIRCLE('',#1880,4.);
#781=CIRCLE('',#1882,4.);
#782=CIRCLE('',#1884,8.);
#783=CIRCLE('',#1888,2.);
#784=CIRCLE('',#1889,2.);
#785=VERTEX_POINT('',#2475);
#786=VERTEX_POINT('',#2477);
#787=VERTEX_POINT('',#2481);
#788=VERTEX_POINT('',#2483);
#789=VERTEX_POINT('',#2487);
#790=VERTEX_POINT('',#2489);
#791=VERTEX_POINT('',#2493);
#792=VERTEX_POINT('',#2495);
#793=VERTEX_POINT('',#2499);
#794=VERTEX_POINT('',#2501);
#795=VERTEX_POINT('',#2505);
#796=VERTEX_POINT('',#2506);
#797=VERTEX_POINT('',#2508);
#798=VERTEX_POINT('',#2510);
#799=VERTEX_POINT('',#2514);
#800=VERTEX_POINT('',#2516);
#801=VERTEX_POINT('',#2520);
#802=VERTEX_POINT('',#2522);
#803=VERTEX_POINT('',#2532);
#804=VERTEX_POINT('',#2534);
#805=VERTEX_POINT('',#2538);
#806=VERTEX_POINT('',#2540);
#807=VERTEX_POINT('',#2547);
#808=VERTEX_POINT('',#2549);
#809=VERTEX_POINT('',#2553);
#810=VERTEX_POINT('',#2555);
#811=VERTEX_POINT('',#2559);
#812=VERTEX_POINT('',#2561);
#813=VERTEX_POINT('',#2565);
#814=VERTEX_POINT('',#2566);
#815=VERTEX_POINT('',#2568);
#816=VERTEX_POINT('',#2570);
#817=VERTEX_POINT('',#2574);
#818=VERTEX_POINT('',#2576);
#819=VERTEX_POINT('',#2580);
#820=VERTEX_POINT('',#2582);
#821=VERTEX_POINT('',#2592);
#822=VERTEX_POINT('',#2594);
#823=VERTEX_POINT('',#2598);
#824=VERTEX_POINT('',#2600);
#825=VERTEX_POINT('',#2604);
#826=VERTEX_POINT('',#2606);
#827=VERTEX_POINT('',#2610);
#828=VERTEX_POINT('',#2611);
#829=VERTEX_POINT('',#2613);
#830=VERTEX_POINT('',#2615);
#831=VERTEX_POINT('',#2619);
#832=VERTEX_POINT('',#2621);
#833=VERTEX_POINT('',#2625);
#834=VERTEX_POINT('',#2627);
#835=VERTEX_POINT('',#2637);
#836=VERTEX_POINT('',#2639);
#837=VERTEX_POINT('',#2643);
#838=VERTEX_POINT('',#2646);
#839=VERTEX_POINT('',#2649);
#840=VERTEX_POINT('',#2653);
#841=VERTEX_POINT('',#2655);
#842=VERTEX_POINT('',#2658);
#843=VERTEX_POINT('',#2667);
#844=VERTEX_POINT('',#2669);
#845=VERTEX_POINT('',#2673);
#846=VERTEX_POINT('',#2676);
#847=VERTEX_POINT('',#2679);
#848=VERTEX_POINT('',#2683);
#849=VERTEX_POINT('',#2685);
#850=VERTEX_POINT('',#2688);
#851=VERTEX_POINT('',#2692);
#852=VERTEX_POINT('',#2695);
#853=VERTEX_POINT('',#2703);
#854=VERTEX_POINT('',#2705);
#855=VERTEX_POINT('',#2708);
#856=VERTEX_POINT('',#2712);
#857=VERTEX_POINT('',#2715);
#858=VERTEX_POINT('',#2719);
#859=VERTEX_POINT('',#2725);
#860=VERTEX_POINT('',#2727);
#861=VERTEX_POINT('',#2731);
#862=VERTEX_POINT('',#2733);
#863=VERTEX_POINT('',#2737);
#864=VERTEX_POINT('',#2738);
#865=VERTEX_POINT('',#2740);
#866=VERTEX_POINT('',#2742);
#867=VERTEX_POINT('',#2746);
#868=VERTEX_POINT('',#2748);
#869=VERTEX_POINT('',#2752);
#870=VERTEX_POINT('',#2754);
#871=VERTEX_POINT('',#2764);
#872=VERTEX_POINT('',#2766);
#873=VERTEX_POINT('',#2770);
#874=VERTEX_POINT('',#2772);
#875=VERTEX_POINT('',#2779);
#876=VERTEX_POINT('',#2781);
#877=VERTEX_POINT('',#2785);
#878=VERTEX_POINT('',#2788);
#879=VERTEX_POINT('',#2791);
#880=VERTEX_POINT('',#2795);
#881=VERTEX_POINT('',#2797);
#882=VERTEX_POINT('',#2800);
#883=VERTEX_POINT('',#2809);
#884=VERTEX_POINT('',#2811);
#885=VERTEX_POINT('',#2815);
#886=VERTEX_POINT('',#2817);
#887=VERTEX_POINT('',#2824);
#888=VERTEX_POINT('',#2825);
#889=VERTEX_POINT('',#2827);
#890=VERTEX_POINT('',#2829);
#891=VERTEX_POINT('',#2833);
#892=VERTEX_POINT('',#2834);
#893=VERTEX_POINT('',#2836);
#894=VERTEX_POINT('',#2838);
#895=VERTEX_POINT('',#2851);
#896=VERTEX_POINT('',#2853);
#897=VERTEX_POINT('',#2858);
#898=EDGE_CURVE('',#785,#785,#697,.T.);
#899=EDGE_CURVE('',#785,#786,#535,.T.);
#900=EDGE_CURVE('',#786,#786,#698,.T.);
#901=EDGE_CURVE('',#787,#787,#699,.T.);
#902=EDGE_CURVE('',#787,#788,#536,.T.);
#903=EDGE_CURVE('',#788,#788,#700,.T.);
#904=EDGE_CURVE('',#789,#789,#701,.T.);
#905=EDGE_CURVE('',#789,#790,#537,.T.);
#906=EDGE_CURVE('',#790,#790,#702,.T.);
#907=EDGE_CURVE('',#791,#791,#703,.T.);
#908=EDGE_CURVE('',#791,#792,#538,.T.);
#909=EDGE_CURVE('',#792,#792,#704,.T.);
#910=EDGE_CURVE('',#793,#793,#705,.T.);
#911=EDGE_CURVE('',#793,#794,#539,.T.);
#912=EDGE_CURVE('',#794,#794,#706,.T.);
#913=EDGE_CURVE('',#795,#796,#540,.T.);
#914=EDGE_CURVE('',#796,#797,#541,.T.);
#915=EDGE_CURVE('',#798,#797,#542,.T.);
#916=EDGE_CURVE('',#795,#798,#543,.T.);
#917=EDGE_CURVE('',#799,#795,#544,.T.);
#918=EDGE_CURVE('',#800,#798,#545,.T.);
#919=EDGE_CURVE('',#799,#800,#546,.T.);
#920=EDGE_CURVE('',#801,#799,#547,.T.);
#921=EDGE_CURVE('',#802,#800,#548,.T.);
#922=EDGE_CURVE('',#801,#802,#549,.T.);
#923=EDGE_CURVE('',#796,#801,#550,.T.);
#924=EDGE_CURVE('',#797,#802,#551,.T.);
#925=EDGE_CURVE('',#803,#803,#707,.T.);
#926=EDGE_CURVE('',#803,#804,#552,.T.);
#927=EDGE_CURVE('',#804,#804,#708,.T.);
#928=EDGE_CURVE('',#805,#805,#709,.T.);
#929=EDGE_CURVE('',#805,#806,#553,.T.);
#930=EDGE_CURVE('',#806,#806,#710,.T.);
#931=EDGE_CURVE('',#807,#807,#711,.T.);
#932=EDGE_CURVE('',#807,#808,#554,.T.);
#933=EDGE_CURVE('',#808,#808,#712,.T.);
#934=EDGE_CURVE('',#809,#809,#713,.T.);
#935=EDGE_CURVE('',#809,#810,#555,.T.);
#936=EDGE_CURVE('',#810,#810,#714,.T.);
#937=EDGE_CURVE('',#811,#811,#715,.T.);
#938=EDGE_CURVE('',#811,#812,#556,.T.);
#939=EDGE_CURVE('',#812,#812,#716,.T.);
#940=EDGE_CURVE('',#813,#814,#557,.T.);
#941=EDGE_CURVE('',#814,#815,#558,.T.);
#942=EDGE_CURVE('',#816,#815,#559,.T.);
#943=EDGE_CURVE('',#813,#816,#560,.T.);
#944=EDGE_CURVE('',#817,#813,#717,.T.);
#945=EDGE_CURVE('',#818,#816,#718,.T.);
#946=EDGE_CURVE('',#817,#818,#561,.T.);
#947=EDGE_CURVE('',#819,#817,#562,.T.);
#948=EDGE_CURVE('',#820,#818,#563,.T.);
#949=EDGE_CURVE('',#819,#820,#564,.T.);
#950=EDGE_CURVE('',#814,#819,#719,.T.);
#951=EDGE_CURVE('',#815,#820,#720,.T.);
#952=EDGE_CURVE('',#821,#821,#721,.T.);
#953=EDGE_CURVE('',#821,#822,#565,.T.);
#954=EDGE_CURVE('',#822,#822,#722,.T.);
#955=EDGE_CURVE('',#823,#823,#723,.T.);
#956=EDGE_CURVE('',#823,#824,#566,.T.);
#957=EDGE_CURVE('',#824,#824,#724,.T.);
#958=EDGE_CURVE('',#825,#825,#725,.T.);
#959=EDGE_CURVE('',#825,#826,#567,.T.);
#960=EDGE_CURVE('',#826,#826,#726,.T.);
#961=EDGE_CURVE('',#827,#828,#568,.T.);
#962=EDGE_CURVE('',#828,#829,#569,.T.);
#963=EDGE_CURVE('',#830,#829,#570,.T.);
#964=EDGE_CURVE('',#827,#830,#571,.T.);
#965=EDGE_CURVE('',#831,#827,#727,.T.);
#966=EDGE_CURVE('',#832,#830,#728,.T.);
#967=EDGE_CURVE('',#831,#832,#572,.T.);
#968=EDGE_CURVE('',#833,#831,#573,.T.);
#969=EDGE_CURVE('',#834,#832,#574,.T.);
#970=EDGE_CURVE('',#833,#834,#575,.T.);
#971=EDGE_CURVE('',#828,#833,#729,.T.);
#972=EDGE_CURVE('',#829,#834,#730,.T.);
#973=EDGE_CURVE('',#835,#835,#731,.T.);
#974=EDGE_CURVE('',#835,#836,#576,.T.);
#975=EDGE_CURVE('',#836,#836,#732,.T.);
#976=EDGE_CURVE('',#837,#837,#733,.T.);
#977=EDGE_CURVE('',#838,#838,#734,.T.);
#978=EDGE_CURVE('',#839,#839,#735,.T.);
#979=EDGE_CURVE('',#839,#838,#577,.T.);
#980=EDGE_CURVE('',#840,#840,#736,.T.);
#981=EDGE_CURVE('',#841,#841,#737,.T.);
#982=EDGE_CURVE('',#840,#842,#578,.T.);
#983=EDGE_CURVE('',#842,#842,#738,.T.);
#984=EDGE_CURVE('',#837,#841,#579,.T.);
#985=EDGE_CURVE('',#843,#843,#739,.T.);
#986=EDGE_CURVE('',#843,#844,#580,.T.);
#987=EDGE_CURVE('',#844,#844,#740,.T.);
#988=EDGE_CURVE('',#845,#845,#741,.T.);
#989=EDGE_CURVE('',#846,#846,#742,.T.);
#990=EDGE_CURVE('',#847,#847,#743,.T.);
#991=EDGE_CURVE('',#847,#846,#581,.T.);
#992=EDGE_CURVE('',#848,#848,#744,.T.);
#993=EDGE_CURVE('',#849,#849,#745,.T.);
#994=EDGE_CURVE('',#848,#850,#582,.T.);
#995=EDGE_CURVE('',#850,#850,#746,.T.);
#996=EDGE_CURVE('',#851,#851,#747,.T.);
#997=EDGE_CURVE('',#852,#852,#748,.T.);
#998=EDGE_CURVE('',#852,#851,#583,.T.);
#999=EDGE_CURVE('',#845,#849,#584,.T.);
#1000=EDGE_CURVE('',#853,#853,#749,.T.);
#1001=EDGE_CURVE('',#854,#854,#750,.T.);
#1002=EDGE_CURVE('',#855,#855,#751,.T.);
#1003=EDGE_CURVE('',#855,#853,#585,.T.);
#1004=EDGE_CURVE('',#856,#856,#752,.T.);
#1005=EDGE_CURVE('',#856,#857,#586,.T.);
#1006=EDGE_CURVE('',#857,#857,#753,.T.);
#1007=EDGE_CURVE('',#854,#858,#587,.T.);
#1008=EDGE_CURVE('',#858,#858,#754,.T.);
#1009=EDGE_CURVE('',#859,#859,#755,.T.);
#1010=EDGE_CURVE('',#859,#860,#588,.T.);
#1011=EDGE_CURVE('',#860,#860,#756,.T.);
#1012=EDGE_CURVE('',#861,#861,#757,.T.);
#1013=EDGE_CURVE('',#861,#862,#589,.T.);
#1014=EDGE_CURVE('',#862,#862,#758,.T.);
#1015=EDGE_CURVE('',#863,#864,#590,.T.);
#1016=EDGE_CURVE('',#864,#865,#591,.T.);
#1017=EDGE_CURVE('',#866,#865,#592,.T.);
#1018=EDGE_CURVE('',#863,#866,#593,.T.);
#1019=EDGE_CURVE('',#867,#863,#759,.T.);
#1020=EDGE_CURVE('',#868,#866,#760,.T.);
#1021=EDGE_CURVE('',#867,#868,#594,.T.);
#1022=EDGE_CURVE('',#869,#867,#595,.T.);
#1023=EDGE_CURVE('',#870,#868,#596,.T.);
#1024=EDGE_CURVE('',#869,#870,#597,.T.);
#1025=EDGE_CURVE('',#864,#869,#761,.T.);
#1026=EDGE_CURVE('',#865,#870,#762,.T.);
#1027=EDGE_CURVE('',#871,#871,#763,.T.);
#1028=EDGE_CURVE('',#871,#872,#598,.T.);
#1029=EDGE_CURVE('',#872,#872,#764,.T.);
#1030=EDGE_CURVE('',#873,#873,#765,.T.);
#1031=EDGE_CURVE('',#873,#874,#599,.T.);
#1032=EDGE_CURVE('',#874,#874,#766,.T.);
#1033=EDGE_CURVE('',#875,#875,#767,.T.);
#1034=EDGE_CURVE('',#875,#876,#600,.T.);
#1035=EDGE_CURVE('',#876,#876,#768,.T.);
#1036=EDGE_CURVE('',#877,#877,#769,.T.);
#1037=EDGE_CURVE('',#878,#878,#770,.T.);
#1038=EDGE_CURVE('',#879,#879,#771,.T.);
#1039=EDGE_CURVE('',#879,#878,#601,.T.);
#1040=EDGE_CURVE('',#880,#880,#772,.T.);
#1041=EDGE_CURVE('',#881,#881,#773,.T.);
#1042=EDGE_CURVE('',#880,#882,#602,.T.);
#1043=EDGE_CURVE('',#882,#882,#774,.T.);
#1044=EDGE_CURVE('',#877,#881,#603,.T.);
#1045=EDGE_CURVE('',#883,#883,#775,.T.);
#1046=EDGE_CURVE('',#883,#884,#604,.T.);
#1047=EDGE_CURVE('',#884,#884,#776,.T.);
#1048=EDGE_CURVE('',#885,#885,#777,.T.);
#1049=EDGE_CURVE('',#885,#886,#605,.T.);
#1050=EDGE_CURVE('',#886,#886,#778,.T.);
#1051=EDGE_CURVE('',#887,#888,#606,.T.);
#1052=EDGE_CURVE('',#889,#887,#607,.T.);
#1053=EDGE_CURVE('',#890,#889,#608,.T.);
#1054=EDGE_CURVE('',#888,#890,#609,.T.);
#1055=EDGE_CURVE('',#891,#892,#610,.T.);
#1056=EDGE_CURVE('',#893,#891,#611,.T.);
#1057=EDGE_CURVE('',#894,#893,#612,.T.);
#1058=EDGE_CURVE('',#892,#894,#613,.T.);
#1059=EDGE_CURVE('',#889,#894,#779,.T.);
#1060=EDGE_CURVE('',#892,#887,#780,.T.);
#1061=EDGE_CURVE('',#891,#888,#781,.T.);
#1062=EDGE_CURVE('',#890,#893,#782,.T.);
#1063=EDGE_CURVE('',#895,#895,#783,.T.);
#1064=EDGE_CURVE('',#895,#896,#614,.T.);
#1065=EDGE_CURVE('',#896,#896,#784,.T.);
#1066=EDGE_CURVE('',#896,#897,#615,.T.);
#1067=ORIENTED_EDGE('',*,*,#898,.F.);
#1068=ORIENTED_EDGE('',*,*,#899,.T.);
#1069=ORIENTED_EDGE('',*,*,#900,.F.);
#1070=ORIENTED_EDGE('',*,*,#899,.F.);
#1071=ORIENTED_EDGE('',*,*,#901,.F.);
#1072=ORIENTED_EDGE('',*,*,#902,.T.);
#1073=ORIENTED_EDGE('',*,*,#903,.F.);
#1074=ORIENTED_EDGE('',*,*,#902,.F.);
#1075=ORIENTED_EDGE('',*,*,#904,.F.);
#1076=ORIENTED_EDGE('',*,*,#905,.T.);
#1077=ORIENTED_EDGE('',*,*,#906,.F.);
#1078=ORIENTED_EDGE('',*,*,#905,.F.);
#1079=ORIENTED_EDGE('',*,*,#907,.F.);
#1080=ORIENTED_EDGE('',*,*,#908,.T.);
#1081=ORIENTED_EDGE('',*,*,#909,.F.);
#1082=ORIENTED_EDGE('',*,*,#908,.F.);
#1083=ORIENTED_EDGE('',*,*,#910,.F.);
#1084=ORIENTED_EDGE('',*,*,#911,.T.);
#1085=ORIENTED_EDGE('',*,*,#912,.F.);
#1086=ORIENTED_EDGE('',*,*,#911,.F.);
#1087=ORIENTED_EDGE('',*,*,#913,.T.);
#1088=ORIENTED_EDGE('',*,*,#914,.T.);
#1089=ORIENTED_EDGE('',*,*,#915,.F.);
#1090=ORIENTED_EDGE('',*,*,#916,.F.);
#1091=ORIENTED_EDGE('',*,*,#917,.T.);
#1092=ORIENTED_EDGE('',*,*,#916,.T.);
#1093=ORIENTED_EDGE('',*,*,#918,.F.);
#1094=ORIENTED_EDGE('',*,*,#919,.F.);
#1095=ORIENTED_EDGE('',*,*,#920,.T.);
#1096=ORIENTED_EDGE('',*,*,#919,.T.);
#1097=ORIENTED_EDGE('',*,*,#921,.F.);
#1098=ORIENTED_EDGE('',*,*,#922,.F.);
#1099=ORIENTED_EDGE('',*,*,#923,.T.);
#1100=ORIENTED_EDGE('',*,*,#922,.T.);
#1101=ORIENTED_EDGE('',*,*,#924,.F.);
#1102=ORIENTED_EDGE('',*,*,#914,.F.);
#1103=ORIENTED_EDGE('',*,*,#924,.T.);
#1104=ORIENTED_EDGE('',*,*,#921,.T.);
#1105=ORIENTED_EDGE('',*,*,#918,.T.);
#1106=ORIENTED_EDGE('',*,*,#915,.T.);
#1107=ORIENTED_EDGE('',*,*,#910,.T.);
#1108=ORIENTED_EDGE('',*,*,#907,.T.);
#1109=ORIENTED_EDGE('',*,*,#904,.T.);
#1110=ORIENTED_EDGE('',*,*,#901,.T.);
#1111=ORIENTED_EDGE('',*,*,#898,.T.);
#1112=ORIENTED_EDGE('',*,*,#923,.F.);
#1113=ORIENTED_EDGE('',*,*,#913,.F.);
#1114=ORIENTED_EDGE('',*,*,#917,.F.);
#1115=ORIENTED_EDGE('',*,*,#920,.F.);
#1116=ORIENTED_EDGE('',*,*,#912,.T.);
#1117=ORIENTED_EDGE('',*,*,#909,.T.);
#1118=ORIENTED_EDGE('',*,*,#906,.T.);
#1119=ORIENTED_EDGE('',*,*,#903,.T.);
#1120=ORIENTED_EDGE('',*,*,#900,.T.);
#1121=ORIENTED_EDGE('',*,*,#925,.F.);
#1122=ORIENTED_EDGE('',*,*,#926,.T.);
#1123=ORIENTED_EDGE('',*,*,#927,.T.);
#1124=ORIENTED_EDGE('',*,*,#926,.F.);
#1125=ORIENTED_EDGE('',*,*,#928,.F.);
#1126=ORIENTED_EDGE('',*,*,#929,.T.);
#1127=ORIENTED_EDGE('',*,*,#930,.T.);
#1128=ORIENTED_EDGE('',*,*,#929,.F.);
#1129=ORIENTED_EDGE('',*,*,#928,.T.);
#1130=ORIENTED_EDGE('',*,*,#925,.T.);
#1131=ORIENTED_EDGE('',*,*,#930,.F.);
#1132=ORIENTED_EDGE('',*,*,#927,.F.);
#1133=ORIENTED_EDGE('',*,*,#931,.F.);
#1134=ORIENTED_EDGE('',*,*,#932,.T.);
#1135=ORIENTED_EDGE('',*,*,#933,.F.);
#1136=ORIENTED_EDGE('',*,*,#932,.F.);
#1137=ORIENTED_EDGE('',*,*,#934,.F.);
#1138=ORIENTED_EDGE('',*,*,#935,.T.);
#1139=ORIENTED_EDGE('',*,*,#936,.F.);
#1140=ORIENTED_EDGE('',*,*,#935,.F.);
#1141=ORIENTED_EDGE('',*,*,#937,.F.);
#1142=ORIENTED_EDGE('',*,*,#938,.T.);
#1143=ORIENTED_EDGE('',*,*,#939,.F.);
#1144=ORIENTED_EDGE('',*,*,#938,.F.);
#1145=ORIENTED_EDGE('',*,*,#940,.T.);
#1146=ORIENTED_EDGE('',*,*,#941,.T.);
#1147=ORIENTED_EDGE('',*,*,#942,.F.);
#1148=ORIENTED_EDGE('',*,*,#943,.F.);
#1149=ORIENTED_EDGE('',*,*,#944,.T.);
#1150=ORIENTED_EDGE('',*,*,#943,.T.);
#1151=ORIENTED_EDGE('',*,*,#945,.F.);
#1152=ORIENTED_EDGE('',*,*,#946,.F.);
#1153=ORIENTED_EDGE('',*,*,#947,.T.);
#1154=ORIENTED_EDGE('',*,*,#946,.T.);
#1155=ORIENTED_EDGE('',*,*,#948,.F.);
#1156=ORIENTED_EDGE('',*,*,#949,.F.);
#1157=ORIENTED_EDGE('',*,*,#950,.T.);
#1158=ORIENTED_EDGE('',*,*,#949,.T.);
#1159=ORIENTED_EDGE('',*,*,#951,.F.);
#1160=ORIENTED_EDGE('',*,*,#941,.F.);
#1161=ORIENTED_EDGE('',*,*,#951,.T.);
#1162=ORIENTED_EDGE('',*,*,#948,.T.);
#1163=ORIENTED_EDGE('',*,*,#945,.T.);
#1164=ORIENTED_EDGE('',*,*,#942,.T.);
#1165=ORIENTED_EDGE('',*,*,#931,.T.);
#1166=ORIENTED_EDGE('',*,*,#934,.T.);
#1167=ORIENTED_EDGE('',*,*,#937,.T.);
#1168=ORIENTED_EDGE('',*,*,#950,.F.);
#1169=ORIENTED_EDGE('',*,*,#940,.F.);
#1170=ORIENTED_EDGE('',*,*,#944,.F.);
#1171=ORIENTED_EDGE('',*,*,#947,.F.);
#1172=ORIENTED_EDGE('',*,*,#933,.T.);
#1173=ORIENTED_EDGE('',*,*,#936,.T.);
#1174=ORIENTED_EDGE('',*,*,#939,.T.);
#1175=ORIENTED_EDGE('',*,*,#952,.F.);
#1176=ORIENTED_EDGE('',*,*,#953,.T.);
#1177=ORIENTED_EDGE('',*,*,#954,.F.);
#1178=ORIENTED_EDGE('',*,*,#953,.F.);
#1179=ORIENTED_EDGE('',*,*,#955,.F.);
#1180=ORIENTED_EDGE('',*,*,#956,.T.);
#1181=ORIENTED_EDGE('',*,*,#957,.F.);
#1182=ORIENTED_EDGE('',*,*,#956,.F.);
#1183=ORIENTED_EDGE('',*,*,#958,.F.);
#1184=ORIENTED_EDGE('',*,*,#959,.T.);
#1185=ORIENTED_EDGE('',*,*,#960,.F.);
#1186=ORIENTED_EDGE('',*,*,#959,.F.);
#1187=ORIENTED_EDGE('',*,*,#961,.T.);
#1188=ORIENTED_EDGE('',*,*,#962,.T.);
#1189=ORIENTED_EDGE('',*,*,#963,.F.);
#1190=ORIENTED_EDGE('',*,*,#964,.F.);
#1191=ORIENTED_EDGE('',*,*,#965,.T.);
#1192=ORIENTED_EDGE('',*,*,#964,.T.);
#1193=ORIENTED_EDGE('',*,*,#966,.F.);
#1194=ORIENTED_EDGE('',*,*,#967,.F.);
#1195=ORIENTED_EDGE('',*,*,#968,.T.);
#1196=ORIENTED_EDGE('',*,*,#967,.T.);
#1197=ORIENTED_EDGE('',*,*,#969,.F.);
#1198=ORIENTED_EDGE('',*,*,#970,.F.);
#1199=ORIENTED_EDGE('',*,*,#971,.T.);
#1200=ORIENTED_EDGE('',*,*,#970,.T.);
#1201=ORIENTED_EDGE('',*,*,#972,.F.);
#1202=ORIENTED_EDGE('',*,*,#962,.F.);
#1203=ORIENTED_EDGE('',*,*,#972,.T.);
#1204=ORIENTED_EDGE('',*,*,#969,.T.);
#1205=ORIENTED_EDGE('',*,*,#966,.T.);
#1206=ORIENTED_EDGE('',*,*,#963,.T.);
#1207=ORIENTED_EDGE('',*,*,#952,.T.);
#1208=ORIENTED_EDGE('',*,*,#955,.T.);
#1209=ORIENTED_EDGE('',*,*,#958,.T.);
#1210=ORIENTED_EDGE('',*,*,#971,.F.);
#1211=ORIENTED_EDGE('',*,*,#961,.F.);
#1212=ORIENTED_EDGE('',*,*,#965,.F.);
#1213=ORIENTED_EDGE('',*,*,#968,.F.);
#1214=ORIENTED_EDGE('',*,*,#954,.T.);
#1215=ORIENTED_EDGE('',*,*,#957,.T.);
#1216=ORIENTED_EDGE('',*,*,#960,.T.);
#1217=ORIENTED_EDGE('',*,*,#973,.T.);
#1218=ORIENTED_EDGE('',*,*,#974,.T.);
#1219=ORIENTED_EDGE('',*,*,#975,.F.);
#1220=ORIENTED_EDGE('',*,*,#974,.F.);
#1221=ORIENTED_EDGE('',*,*,#976,.F.);
#1222=ORIENTED_EDGE('',*,*,#973,.F.);
#1223=ORIENTED_EDGE('',*,*,#977,.F.);
#1224=ORIENTED_EDGE('',*,*,#975,.T.);
#1225=ORIENTED_EDGE('',*,*,#978,.F.);
#1226=ORIENTED_EDGE('',*,*,#979,.T.);
#1227=ORIENTED_EDGE('',*,*,#977,.T.);
#1228=ORIENTED_EDGE('',*,*,#979,.F.);
#1229=ORIENTED_EDGE('',*,*,#980,.T.);
#1230=ORIENTED_EDGE('',*,*,#981,.F.);
#1231=ORIENTED_EDGE('',*,*,#980,.F.);
#1232=ORIENTED_EDGE('',*,*,#982,.T.);
#1233=ORIENTED_EDGE('',*,*,#983,.T.);
#1234=ORIENTED_EDGE('',*,*,#982,.F.);
#1235=ORIENTED_EDGE('',*,*,#983,.F.);
#1236=ORIENTED_EDGE('',*,*,#976,.T.);
#1237=ORIENTED_EDGE('',*,*,#984,.T.);
#1238=ORIENTED_EDGE('',*,*,#981,.T.);
#1239=ORIENTED_EDGE('',*,*,#984,.F.);
#1240=ORIENTED_EDGE('',*,*,#978,.T.);
#1241=ORIENTED_EDGE('',*,*,#985,.T.);
#1242=ORIENTED_EDGE('',*,*,#986,.T.);
#1243=ORIENTED_EDGE('',*,*,#987,.F.);
#1244=ORIENTED_EDGE('',*,*,#986,.F.);
#1245=ORIENTED_EDGE('',*,*,#988,.F.);
#1246=ORIENTED_EDGE('',*,*,#985,.F.);
#1247=ORIENTED_EDGE('',*,*,#989,.F.);
#1248=ORIENTED_EDGE('',*,*,#987,.T.);
#1249=ORIENTED_EDGE('',*,*,#990,.F.);
#1250=ORIENTED_EDGE('',*,*,#991,.T.);
#1251=ORIENTED_EDGE('',*,*,#989,.T.);
#1252=ORIENTED_EDGE('',*,*,#991,.F.);
#1253=ORIENTED_EDGE('',*,*,#992,.T.);
#1254=ORIENTED_EDGE('',*,*,#993,.F.);
#1255=ORIENTED_EDGE('',*,*,#992,.F.);
#1256=ORIENTED_EDGE('',*,*,#994,.T.);
#1257=ORIENTED_EDGE('',*,*,#995,.T.);
#1258=ORIENTED_EDGE('',*,*,#994,.F.);
#1259=ORIENTED_EDGE('',*,*,#995,.F.);
#1260=ORIENTED_EDGE('',*,*,#996,.F.);
#1261=ORIENTED_EDGE('',*,*,#997,.F.);
#1262=ORIENTED_EDGE('',*,*,#998,.T.);
#1263=ORIENTED_EDGE('',*,*,#996,.T.);
#1264=ORIENTED_EDGE('',*,*,#998,.F.);
#1265=ORIENTED_EDGE('',*,*,#988,.T.);
#1266=ORIENTED_EDGE('',*,*,#999,.T.);
#1267=ORIENTED_EDGE('',*,*,#993,.T.);
#1268=ORIENTED_EDGE('',*,*,#999,.F.);
#1269=ORIENTED_EDGE('',*,*,#990,.T.);
#1270=ORIENTED_EDGE('',*,*,#997,.T.);
#1271=ORIENTED_EDGE('',*,*,#1000,.F.);
#1272=ORIENTED_EDGE('',*,*,#1001,.T.);
#1273=ORIENTED_EDGE('',*,*,#1002,.F.);
#1274=ORIENTED_EDGE('',*,*,#1003,.T.);
#1275=ORIENTED_EDGE('',*,*,#1000,.T.);
#1276=ORIENTED_EDGE('',*,*,#1003,.F.);
#1277=ORIENTED_EDGE('',*,*,#1002,.T.);
#1278=ORIENTED_EDGE('',*,*,#1004,.T.);
#1279=ORIENTED_EDGE('',*,*,#1004,.F.);
#1280=ORIENTED_EDGE('',*,*,#1005,.T.);
#1281=ORIENTED_EDGE('',*,*,#1006,.T.);
#1282=ORIENTED_EDGE('',*,*,#1005,.F.);
#1283=ORIENTED_EDGE('',*,*,#1001,.F.);
#1284=ORIENTED_EDGE('',*,*,#1007,.T.);
#1285=ORIENTED_EDGE('',*,*,#1008,.T.);
#1286=ORIENTED_EDGE('',*,*,#1007,.F.);
#1287=ORIENTED_EDGE('',*,*,#1008,.F.);
#1288=ORIENTED_EDGE('',*,*,#1006,.F.);
#1289=ORIENTED_EDGE('',*,*,#1009,.F.);
#1290=ORIENTED_EDGE('',*,*,#1010,.T.);
#1291=ORIENTED_EDGE('',*,*,#1011,.F.);
#1292=ORIENTED_EDGE('',*,*,#1010,.F.);
#1293=ORIENTED_EDGE('',*,*,#1012,.F.);
#1294=ORIENTED_EDGE('',*,*,#1013,.T.);
#1295=ORIENTED_EDGE('',*,*,#1014,.F.);
#1296=ORIENTED_EDGE('',*,*,#1013,.F.);
#1297=ORIENTED_EDGE('',*,*,#1015,.T.);
#1298=ORIENTED_EDGE('',*,*,#1016,.T.);
#1299=ORIENTED_EDGE('',*,*,#1017,.F.);
#1300=ORIENTED_EDGE('',*,*,#1018,.F.);
#1301=ORIENTED_EDGE('',*,*,#1019,.T.);
#1302=ORIENTED_EDGE('',*,*,#1018,.T.);
#1303=ORIENTED_EDGE('',*,*,#1020,.F.);
#1304=ORIENTED_EDGE('',*,*,#1021,.F.);
#1305=ORIENTED_EDGE('',*,*,#1022,.T.);
#1306=ORIENTED_EDGE('',*,*,#1021,.T.);
#1307=ORIENTED_EDGE('',*,*,#1023,.F.);
#1308=ORIENTED_EDGE('',*,*,#1024,.F.);
#1309=ORIENTED_EDGE('',*,*,#1025,.T.);
#1310=ORIENTED_EDGE('',*,*,#1024,.T.);
#1311=ORIENTED_EDGE('',*,*,#1026,.F.);
#1312=ORIENTED_EDGE('',*,*,#1016,.F.);
#1313=ORIENTED_EDGE('',*,*,#1026,.T.);
#1314=ORIENTED_EDGE('',*,*,#1023,.T.);
#1315=ORIENTED_EDGE('',*,*,#1020,.T.);
#1316=ORIENTED_EDGE('',*,*,#1017,.T.);
#1317=ORIENTED_EDGE('',*,*,#1009,.T.);
#1318=ORIENTED_EDGE('',*,*,#1012,.T.);
#1319=ORIENTED_EDGE('',*,*,#1025,.F.);
#1320=ORIENTED_EDGE('',*,*,#1015,.F.);
#1321=ORIENTED_EDGE('',*,*,#1019,.F.);
#1322=ORIENTED_EDGE('',*,*,#1022,.F.);
#1323=ORIENTED_EDGE('',*,*,#1011,.T.);
#1324=ORIENTED_EDGE('',*,*,#1014,.T.);
#1325=ORIENTED_EDGE('',*,*,#1027,.F.);
#1326=ORIENTED_EDGE('',*,*,#1028,.T.);
#1327=ORIENTED_EDGE('',*,*,#1029,.T.);
#1328=ORIENTED_EDGE('',*,*,#1028,.F.);
#1329=ORIENTED_EDGE('',*,*,#1030,.F.);
#1330=ORIENTED_EDGE('',*,*,#1031,.T.);
#1331=ORIENTED_EDGE('',*,*,#1032,.T.);
#1332=ORIENTED_EDGE('',*,*,#1031,.F.);
#1333=ORIENTED_EDGE('',*,*,#1030,.T.);
#1334=ORIENTED_EDGE('',*,*,#1027,.T.);
#1335=ORIENTED_EDGE('',*,*,#1032,.F.);
#1336=ORIENTED_EDGE('',*,*,#1029,.F.);
#1337=ORIENTED_EDGE('',*,*,#1033,.T.);
#1338=ORIENTED_EDGE('',*,*,#1034,.T.);
#1339=ORIENTED_EDGE('',*,*,#1035,.F.);
#1340=ORIENTED_EDGE('',*,*,#1034,.F.);
#1341=ORIENTED_EDGE('',*,*,#1036,.F.);
#1342=ORIENTED_EDGE('',*,*,#1033,.F.);
#1343=ORIENTED_EDGE('',*,*,#1037,.F.);
#1344=ORIENTED_EDGE('',*,*,#1035,.T.);
#1345=ORIENTED_EDGE('',*,*,#1038,.F.);
#1346=ORIENTED_EDGE('',*,*,#1039,.T.);
#1347=ORIENTED_EDGE('',*,*,#1037,.T.);
#1348=ORIENTED_EDGE('',*,*,#1039,.F.);
#1349=ORIENTED_EDGE('',*,*,#1040,.T.);
#1350=ORIENTED_EDGE('',*,*,#1041,.F.);
#1351=ORIENTED_EDGE('',*,*,#1040,.F.);
#1352=ORIENTED_EDGE('',*,*,#1042,.T.);
#1353=ORIENTED_EDGE('',*,*,#1043,.T.);
#1354=ORIENTED_EDGE('',*,*,#1042,.F.);
#1355=ORIENTED_EDGE('',*,*,#1043,.F.);
#1356=ORIENTED_EDGE('',*,*,#1036,.T.);
#1357=ORIENTED_EDGE('',*,*,#1044,.T.);
#1358=ORIENTED_EDGE('',*,*,#1041,.T.);
#1359=ORIENTED_EDGE('',*,*,#1044,.F.);
#1360=ORIENTED_EDGE('',*,*,#1038,.T.);
#1361=ORIENTED_EDGE('',*,*,#1045,.F.);
#1362=ORIENTED_EDGE('',*,*,#1046,.T.);
#1363=ORIENTED_EDGE('',*,*,#1047,.T.);
#1364=ORIENTED_EDGE('',*,*,#1046,.F.);
#1365=ORIENTED_EDGE('',*,*,#1048,.F.);
#1366=ORIENTED_EDGE('',*,*,#1049,.T.);
#1367=ORIENTED_EDGE('',*,*,#1050,.T.);
#1368=ORIENTED_EDGE('',*,*,#1049,.F.);
#1369=ORIENTED_EDGE('',*,*,#1048,.T.);
#1370=ORIENTED_EDGE('',*,*,#1045,.T.);
#1371=ORIENTED_EDGE('',*,*,#1050,.F.);
#1372=ORIENTED_EDGE('',*,*,#1047,.F.);
#1373=ORIENTED_EDGE('',*,*,#1051,.F.);
#1374=ORIENTED_EDGE('',*,*,#1052,.F.);
#1375=ORIENTED_EDGE('',*,*,#1053,.F.);
#1376=ORIENTED_EDGE('',*,*,#1054,.F.);
#1377=ORIENTED_EDGE('',*,*,#1055,.F.);
#1378=ORIENTED_EDGE('',*,*,#1056,.F.);
#1379=ORIENTED_EDGE('',*,*,#1057,.F.);
#1380=ORIENTED_EDGE('',*,*,#1058,.F.);
#1381=ORIENTED_EDGE('',*,*,#1058,.T.);
#1382=ORIENTED_EDGE('',*,*,#1059,.F.);
#1383=ORIENTED_EDGE('',*,*,#1052,.T.);
#1384=ORIENTED_EDGE('',*,*,#1060,.F.);
#1385=ORIENTED_EDGE('',*,*,#1055,.T.);
#1386=ORIENTED_EDGE('',*,*,#1060,.T.);
#1387=ORIENTED_EDGE('',*,*,#1051,.T.);
#1388=ORIENTED_EDGE('',*,*,#1061,.F.);
#1389=ORIENTED_EDGE('',*,*,#1057,.T.);
#1390=ORIENTED_EDGE('',*,*,#1062,.F.);
#1391=ORIENTED_EDGE('',*,*,#1053,.T.);
#1392=ORIENTED_EDGE('',*,*,#1059,.T.);
#1393=ORIENTED_EDGE('',*,*,#1056,.T.);
#1394=ORIENTED_EDGE('',*,*,#1061,.T.);
#1395=ORIENTED_EDGE('',*,*,#1054,.T.);
#1396=ORIENTED_EDGE('',*,*,#1062,.T.);
#1397=ORIENTED_EDGE('',*,*,#1063,.F.);
#1398=ORIENTED_EDGE('',*,*,#1064,.T.);
#1399=ORIENTED_EDGE('',*,*,#1065,.T.);
#1400=ORIENTED_EDGE('',*,*,#1064,.F.);
#1401=ORIENTED_EDGE('',*,*,#1063,.T.);
#1402=ORIENTED_EDGE('',*,*,#1065,.F.);
#1403=ORIENTED_EDGE('',*,*,#1066,.T.);
#1404=ORIENTED_EDGE('',*,*,#1066,.F.);
#1405=CYLINDRICAL_SURFACE('',#1700,4.5);
#1406=CYLINDRICAL_SURFACE('',#1703,4.5);
#1407=CYLINDRICAL_SURFACE('',#1706,4.5);
#1408=CYLINDRICAL_SURFACE('',#1709,4.5);
#1409=CYLINDRICAL_SURFACE('',#1712,5.);
#1410=CYLINDRICAL_SURFACE('',#1722,5.);
#1411=CYLINDRICAL_SURFACE('',#1725,12.);
#1412=CYLINDRICAL_SURFACE('',#1731,7.);
#1413=CYLINDRICAL_SURFACE('',#1734,7.);
#1414=CYLINDRICAL_SURFACE('',#1737,7.);
#1415=CYLINDRICAL_SURFACE('',#1741,12.);
#1416=CYLINDRICAL_SURFACE('',#1745,12.);
#1417=CYLINDRICAL_SURFACE('',#1751,6.);
#1418=CYLINDRICAL_SURFACE('',#1754,7.);
#1419=CYLINDRICAL_SURFACE('',#1757,7.);
#1420=CYLINDRICAL_SURFACE('',#1761,12.);
#1421=CYLINDRICAL_SURFACE('',#1765,12.);
#1422=CYLINDRICAL_SURFACE('',#1771,4.);
#1423=CYLINDRICAL_SURFACE('',#1778,5.);
#1424=CYLINDRICAL_SURFACE('',#1783,8.);
#1425=CYLINDRICAL_SURFACE('',#1786,5.);
#1426=CYLINDRICAL_SURFACE('',#1789,4.);
#1427=CYLINDRICAL_SURFACE('',#1796,5.);
#1428=CYLINDRICAL_SURFACE('',#1801,8.);
#1429=CYLINDRICAL_SURFACE('',#1805,2.);
#1430=CYLINDRICAL_SURFACE('',#1807,5.);
#1431=CYLINDRICAL_SURFACE('',#1813,8.);
#1432=CYLINDRICAL_SURFACE('',#1817,2.);
#1433=CYLINDRICAL_SURFACE('',#1819,6.);
#1434=CYLINDRICAL_SURFACE('',#1823,7.);
#1435=CYLINDRICAL_SURFACE('',#1826,7.);
#1436=CYLINDRICAL_SURFACE('',#1830,12.);
#1437=CYLINDRICAL_SURFACE('',#1834,12.);
#1438=CYLINDRICAL_SURFACE('',#1840,5.);
#1439=CYLINDRICAL_SURFACE('',#1843,7.);
#1440=CYLINDRICAL_SURFACE('',#1849,4.);
#1441=CYLINDRICAL_SURFACE('',#1856,5.);
#1442=CYLINDRICAL_SURFACE('',#1861,8.);
#1443=CYLINDRICAL_SURFACE('',#1864,5.);
#1444=CYLINDRICAL_SURFACE('',#1867,5.);
#1445=CYLINDRICAL_SURFACE('',#1870,10.);
#1446=CYLINDRICAL_SURFACE('',#1881,4.);
#1447=CYLINDRICAL_SURFACE('',#1883,8.);
#1448=CYLINDRICAL_SURFACE('',#1887,2.);
#1449=ADVANCED_FACE('',(#305),#1405,.F.);
#1450=ADVANCED_FACE('',(#306),#1406,.F.);
#1451=ADVANCED_FACE('',(#307),#1407,.F.);
#1452=ADVANCED_FACE('',(#308),#1408,.F.);
#1453=ADVANCED_FACE('',(#309),#1409,.F.);
#1454=ADVANCED_FACE('',(#310),#258,.T.);
#1455=ADVANCED_FACE('',(#311),#259,.T.);
#1456=ADVANCED_FACE('',(#312),#260,.T.);
#1457=ADVANCED_FACE('',(#313),#261,.T.);
#1458=ADVANCED_FACE('',(#314,#212,#213,#214,#215,#216),#262,.T.);
#1459=ADVANCED_FACE('',(#315,#217,#218,#219,#220,#221),#263,.F.);
#1460=ADVANCED_FACE('',(#316),#1410,.F.);
#1461=ADVANCED_FACE('',(#317),#1411,.T.);
#1462=ADVANCED_FACE('',(#318,#222),#264,.T.);
#1463=ADVANCED_FACE('',(#319,#223),#265,.F.);
#1464=ADVANCED_FACE('',(#320),#1412,.F.);
#1465=ADVANCED_FACE('',(#321),#1413,.F.);
#1466=ADVANCED_FACE('',(#322),#1414,.F.);
#1467=ADVANCED_FACE('',(#323),#266,.T.);
#1468=ADVANCED_FACE('',(#324),#1415,.T.);
#1469=ADVANCED_FACE('',(#325),#267,.T.);
#1470=ADVANCED_FACE('',(#326),#1416,.T.);
#1471=ADVANCED_FACE('',(#327,#224,#225,#226),#268,.T.);
#1472=ADVANCED_FACE('',(#328,#227,#228,#229),#269,.F.);
#1473=ADVANCED_FACE('',(#329),#1417,.F.);
#1474=ADVANCED_FACE('',(#330),#1418,.F.);
#1475=ADVANCED_FACE('',(#331),#1419,.F.);
#1476=ADVANCED_FACE('',(#332),#270,.T.);
#1477=ADVANCED_FACE('',(#333),#1420,.T.);
#1478=ADVANCED_FACE('',(#334),#271,.T.);
#1479=ADVANCED_FACE('',(#335),#1421,.T.);
#1480=ADVANCED_FACE('',(#336,#230,#231,#232),#272,.T.);
#1481=ADVANCED_FACE('',(#337,#233,#234,#235),#273,.F.);
#1482=ADVANCED_FACE('',(#338),#1422,.T.);
#1483=ADVANCED_FACE('',(#339,#236),#274,.F.);
#1484=ADVANCED_FACE('',(#340,#237),#275,.F.);
#1485=ADVANCED_FACE('',(#341),#1423,.T.);
#1486=ADVANCED_FACE('',(#342,#238),#276,.T.);
#1487=ADVANCED_FACE('',(#343),#1424,.T.);
#1488=ADVANCED_FACE('',(#344),#277,.F.);
#1489=ADVANCED_FACE('',(#345),#1425,.T.);
#1490=ADVANCED_FACE('',(#346),#278,.T.);
#1491=ADVANCED_FACE('',(#347),#1426,.T.);
#1492=ADVANCED_FACE('',(#348,#239),#279,.F.);
#1493=ADVANCED_FACE('',(#349,#240),#280,.F.);
#1494=ADVANCED_FACE('',(#350),#1427,.T.);
#1495=ADVANCED_FACE('',(#351,#241),#281,.T.);
#1496=ADVANCED_FACE('',(#352),#1428,.T.);
#1497=ADVANCED_FACE('',(#353,#242),#282,.F.);
#1498=ADVANCED_FACE('',(#354),#1429,.F.);
#1499=ADVANCED_FACE('',(#355),#1430,.T.);
#1500=ADVANCED_FACE('',(#356,#243),#283,.T.);
#1501=ADVANCED_FACE('',(#357,#244),#284,.F.);
#1502=ADVANCED_FACE('',(#358),#1431,.T.);
#1503=ADVANCED_FACE('',(#359,#245),#285,.T.);
#1504=ADVANCED_FACE('',(#360),#1432,.F.);
#1505=ADVANCED_FACE('',(#361),#1433,.T.);
#1506=ADVANCED_FACE('',(#362,#246),#286,.F.);
#1507=ADVANCED_FACE('',(#363),#1434,.F.);
#1508=ADVANCED_FACE('',(#364),#1435,.F.);
#1509=ADVANCED_FACE('',(#365),#287,.T.);
#1510=ADVANCED_FACE('',(#366),#1436,.T.);
#1511=ADVANCED_FACE('',(#367),#288,.T.);
#1512=ADVANCED_FACE('',(#368),#1437,.T.);
#1513=ADVANCED_FACE('',(#369,#247,#248),#289,.T.);
#1514=ADVANCED_FACE('',(#370,#249,#250),#290,.F.);
#1515=ADVANCED_FACE('',(#371),#1438,.F.);
#1516=ADVANCED_FACE('',(#372),#1439,.T.);
#1517=ADVANCED_FACE('',(#373,#251),#291,.T.);
#1518=ADVANCED_FACE('',(#374,#252),#292,.F.);
#1519=ADVANCED_FACE('',(#375),#1440,.T.);
#1520=ADVANCED_FACE('',(#376,#253),#293,.F.);
#1521=ADVANCED_FACE('',(#377,#254),#294,.F.);
#1522=ADVANCED_FACE('',(#378),#1441,.T.);
#1523=ADVANCED_FACE('',(#379,#255),#295,.T.);
#1524=ADVANCED_FACE('',(#380),#1442,.T.);
#1525=ADVANCED_FACE('',(#381),#296,.F.);
#1526=ADVANCED_FACE('',(#382),#1443,.T.);
#1527=ADVANCED_FACE('',(#383),#297,.T.);
#1528=ADVANCED_FACE('',(#384),#1444,.F.);
#1529=ADVANCED_FACE('',(#385),#1445,.T.);
#1530=ADVANCED_FACE('',(#386,#256),#298,.T.);
#1531=ADVANCED_FACE('',(#387,#257),#299,.F.);
#1532=ADVANCED_FACE('',(#388),#300,.F.);
#1533=ADVANCED_FACE('',(#389),#301,.F.);
#1534=ADVANCED_FACE('',(#390),#302,.F.);
#1535=ADVANCED_FACE('',(#391),#1446,.F.);
#1536=ADVANCED_FACE('',(#392),#1447,.T.);
#1537=ADVANCED_FACE('',(#393),#303,.T.);
#1538=ADVANCED_FACE('',(#394),#1448,.T.);
#1539=ADVANCED_FACE('',(#395),#304,.T.);
#1540=ADVANCED_FACE('',(#396),#159,.T.);
#1541=CLOSED_SHELL('',(#1449,#1450,#1451,#1452,#1453,#1454,#1455,#1456,
#1457,#1458,#1459));
#1542=CLOSED_SHELL('',(#1460,#1461,#1462,#1463));
#1543=CLOSED_SHELL('',(#1464,#1465,#1466,#1467,#1468,#1469,#1470,#1471,
#1472));
#1544=CLOSED_SHELL('',(#1473,#1474,#1475,#1476,#1477,#1478,#1479,#1480,
#1481));
#1545=CLOSED_SHELL('',(#1482,#1483,#1484,#1485,#1486,#1487,#1488,#1489,
#1490));
#1546=CLOSED_SHELL('',(#1491,#1492,#1493,#1494,#1495,#1496,#1497,#1498,
#1499,#1500));
#1547=CLOSED_SHELL('',(#1501,#1502,#1503,#1504,#1505,#1506));
#1548=CLOSED_SHELL('',(#1507,#1508,#1509,#1510,#1511,#1512,#1513,#1514));
#1549=CLOSED_SHELL('',(#1515,#1516,#1517,#1518));
#1550=CLOSED_SHELL('',(#1519,#1520,#1521,#1522,#1523,#1524,#1525,#1526,
#1527));
#1551=CLOSED_SHELL('',(#1528,#1529,#1530,#1531));
#1552=CLOSED_SHELL('',(#1532,#1533,#1534,#1535,#1536,#1537));
#1553=CLOSED_SHELL('',(#1538,#1539,#1540));
#1554=DERIVED_UNIT_ELEMENT(#1580,1.);
#1555=DERIVED_UNIT_ELEMENT(#2928,-3.);
#1556=DERIVED_UNIT_ELEMENT(#1580,1.);
#1557=DERIVED_UNIT_ELEMENT(#2928,-3.);
#1558=DERIVED_UNIT_ELEMENT(#1580,1.);
#1559=DERIVED_UNIT_ELEMENT(#2928,-3.);
#1560=DERIVED_UNIT_ELEMENT(#1580,1.);
#1561=DERIVED_UNIT_ELEMENT(#2928,-3.);
#1562=DERIVED_UNIT_ELEMENT(#1580,1.);
#1563=DERIVED_UNIT_ELEMENT(#2928,-3.);
#1564=DERIVED_UNIT_ELEMENT(#1580,1.);
#1565=DERIVED_UNIT_ELEMENT(#2928,-3.);
#1566=DERIVED_UNIT_ELEMENT(#1580,1.);
#1567=DERIVED_UNIT_ELEMENT(#2928,-3.);
#1568=DERIVED_UNIT_ELEMENT(#1580,1.);
#1569=DERIVED_UNIT_ELEMENT(#2928,-3.);
#1570=DERIVED_UNIT_ELEMENT(#1580,1.);
#1571=DERIVED_UNIT_ELEMENT(#2928,-3.);
#1572=DERIVED_UNIT_ELEMENT(#1580,1.);
#1573=DERIVED_UNIT_ELEMENT(#2928,-3.);
#1574=DERIVED_UNIT_ELEMENT(#1580,1.);
#1575=DERIVED_UNIT_ELEMENT(#2928,-3.);
#1576=DERIVED_UNIT_ELEMENT(#1580,1.);
#1577=DERIVED_UNIT_ELEMENT(#2928,-3.);
#1578=DERIVED_UNIT_ELEMENT(#1580,1.);
#1579=DERIVED_UNIT_ELEMENT(#2928,-3.);
#1580=(
MASS_UNIT()
NAMED_UNIT(*)
SI_UNIT(.KILO.,.GRAM.)
);
#1581=DERIVED_UNIT((#1554,#1555));
#1582=DERIVED_UNIT((#1556,#1557));
#1583=DERIVED_UNIT((#1558,#1559));
#1584=DERIVED_UNIT((#1560,#1561));
#1585=DERIVED_UNIT((#1562,#1563));
#1586=DERIVED_UNIT((#1564,#1565));
#1587=DERIVED_UNIT((#1566,#1567));
#1588=DERIVED_UNIT((#1568,#1569));
#1589=DERIVED_UNIT((#1570,#1571));
#1590=DERIVED_UNIT((#1572,#1573));
#1591=DERIVED_UNIT((#1574,#1575));
#1592=DERIVED_UNIT((#1576,#1577));
#1593=DERIVED_UNIT((#1578,#1579));
#1594=MEASURE_REPRESENTATION_ITEM('density measure',
POSITIVE_RATIO_MEASURE(7850.),#1581);
#1595=MEASURE_REPRESENTATION_ITEM('density measure',
POSITIVE_RATIO_MEASURE(7850.),#1582);
#1596=MEASURE_REPRESENTATION_ITEM('density measure',
POSITIVE_RATIO_MEASURE(7850.),#1583);
#1597=MEASURE_REPRESENTATION_ITEM('density measure',
POSITIVE_RATIO_MEASURE(7850.),#1584);
#1598=MEASURE_REPRESENTATION_ITEM('density measure',
POSITIVE_RATIO_MEASURE(7850.),#1585);
#1599=MEASURE_REPRESENTATION_ITEM('density measure',
POSITIVE_RATIO_MEASURE(7850.),#1586);
#1600=MEASURE_REPRESENTATION_ITEM('density measure',
POSITIVE_RATIO_MEASURE(7850.),#1587);
#1601=MEASURE_REPRESENTATION_ITEM('density measure',
POSITIVE_RATIO_MEASURE(7850.),#1588);
#1602=MEASURE_REPRESENTATION_ITEM('density measure',
POSITIVE_RATIO_MEASURE(8920.),#1589);
#1603=MEASURE_REPRESENTATION_ITEM('density measure',
POSITIVE_RATIO_MEASURE(7850.),#1590);
#1604=MEASURE_REPRESENTATION_ITEM('density measure',
POSITIVE_RATIO_MEASURE(7850.),#1591);
#1605=MEASURE_REPRESENTATION_ITEM('density measure',
POSITIVE_RATIO_MEASURE(7850.),#1592);
#1606=MEASURE_REPRESENTATION_ITEM('density measure',
POSITIVE_RATIO_MEASURE(7850.),#1593);
#1607=PROPERTY_DEFINITION_REPRESENTATION(#1672,#1633);
#1608=PROPERTY_DEFINITION_REPRESENTATION(#1673,#1634);
#1609=PROPERTY_DEFINITION_REPRESENTATION(#1674,#1635);
#1610=PROPERTY_DEFINITION_REPRESENTATION(#1675,#1636);
#1611=PROPERTY_DEFINITION_REPRESENTATION(#1676,#1637);
#1612=PROPERTY_DEFINITION_REPRESENTATION(#1677,#1638);
#1613=PROPERTY_DEFINITION_REPRESENTATION(#1678,#1639);
#1614=PROPERTY_DEFINITION_REPRESENTATION(#1679,#1640);
#1615=PROPERTY_DEFINITION_REPRESENTATION(#1680,#1641);
#1616=PROPERTY_DEFINITION_REPRESENTATION(#1681,#1642);
#1617=PROPERTY_DEFINITION_REPRESENTATION(#1682,#1643);
#1618=PROPERTY_DEFINITION_REPRESENTATION(#1683,#1644);
#1619=PROPERTY_DEFINITION_REPRESENTATION(#1684,#1645);
#1620=PROPERTY_DEFINITION_REPRESENTATION(#1685,#1646);
#1621=PROPERTY_DEFINITION_REPRESENTATION(#1686,#1647);
#1622=PROPERTY_DEFINITION_REPRESENTATION(#1687,#1648);
#1623=PROPERTY_DEFINITION_REPRESENTATION(#1688,#1649);
#1624=PROPERTY_DEFINITION_REPRESENTATION(#1689,#1650);
#1625=PROPERTY_DEFINITION_REPRESENTATION(#1690,#1651);
#1626=PROPERTY_DEFINITION_REPRESENTATION(#1691,#1652);
#1627=PROPERTY_DEFINITION_REPRESENTATION(#1692,#1653);
#1628=PROPERTY_DEFINITION_REPRESENTATION(#1693,#1654);
#1629=PROPERTY_DEFINITION_REPRESENTATION(#1694,#1655);
#1630=PROPERTY_DEFINITION_REPRESENTATION(#1695,#1656);
#1631=PROPERTY_DEFINITION_REPRESENTATION(#1696,#1657);
#1632=PROPERTY_DEFINITION_REPRESENTATION(#1697,#1658);
#1633=REPRESENTATION('material name',(#1659),#2913);
#1634=REPRESENTATION('density',(#1594),#2913);
#1635=REPRESENTATION('material name',(#1660),#2914);
#1636=REPRESENTATION('density',(#1595),#2914);
#1637=REPRESENTATION('material name',(#1661),#2915);
#1638=REPRESENTATION('density',(#1596),#2915);
#1639=REPRESENTATION('material name',(#1662),#2916);
#1640=REPRESENTATION('density',(#1597),#2916);
#1641=REPRESENTATION('material name',(#1663),#2917);
#1642=REPRESENTATION('density',(#1598),#2917);
#1643=REPRESENTATION('material name',(#1664),#2918);
#1644=REPRESENTATION('density',(#1599),#2918);
#1645=REPRESENTATION('material name',(#1665),#2919);
#1646=REPRESENTATION('density',(#1600),#2919);
#1647=REPRESENTATION('material name',(#1666),#2920);
#1648=REPRESENTATION('density',(#1601),#2920);
#1649=REPRESENTATION('material name',(#1667),#2921);
#1650=REPRESENTATION('density',(#1602),#2921);
#1651=REPRESENTATION('material name',(#1668),#2922);
#1652=REPRESENTATION('density',(#1603),#2922);
#1653=REPRESENTATION('material name',(#1669),#2923);
#1654=REPRESENTATION('density',(#1604),#2923);
#1655=REPRESENTATION('material name',(#1670),#2924);
#1656=REPRESENTATION('density',(#1605),#2924);
#1657=REPRESENTATION('material name',(#1671),#2925);
#1658=REPRESENTATION('density',(#1606),#2925);
#1659=DESCRIPTIVE_REPRESENTATION_ITEM('Steel','Steel');
#1660=DESCRIPTIVE_REPRESENTATION_ITEM('Steel','Steel');
#1661=DESCRIPTIVE_REPRESENTATION_ITEM('Steel','Steel');
#1662=DESCRIPTIVE_REPRESENTATION_ITEM('Steel','Steel');
#1663=DESCRIPTIVE_REPRESENTATION_ITEM('Steel','Steel');
#1664=DESCRIPTIVE_REPRESENTATION_ITEM('Steel','Steel');
#1665=DESCRIPTIVE_REPRESENTATION_ITEM('Steel','Steel');
#1666=DESCRIPTIVE_REPRESENTATION_ITEM('Steel','Steel');
#1667=DESCRIPTIVE_REPRESENTATION_ITEM('Copper, Alloy','Copper, Alloy');
#1668=DESCRIPTIVE_REPRESENTATION_ITEM('Steel','Steel');
#1669=DESCRIPTIVE_REPRESENTATION_ITEM('Steel','Steel');
#1670=DESCRIPTIVE_REPRESENTATION_ITEM('Steel','Steel');
#1671=DESCRIPTIVE_REPRESENTATION_ITEM('Steel','Steel');
#1672=PROPERTY_DEFINITION('material property','material name',#3012);
#1673=PROPERTY_DEFINITION('material property','density of part',#3012);
#1674=PROPERTY_DEFINITION('material property','material name',#3013);
#1675=PROPERTY_DEFINITION('material property','density of part',#3013);
#1676=PROPERTY_DEFINITION('material property','material name',#3014);
#1677=PROPERTY_DEFINITION('material property','density of part',#3014);
#1678=PROPERTY_DEFINITION('material property','material name',#3015);
#1679=PROPERTY_DEFINITION('material property','density of part',#3015);
#1680=PROPERTY_DEFINITION('material property','material name',#3016);
#1681=PROPERTY_DEFINITION('material property','density of part',#3016);
#1682=PROPERTY_DEFINITION('material property','material name',#3017);
#1683=PROPERTY_DEFINITION('material property','density of part',#3017);
#1684=PROPERTY_DEFINITION('material property','material name',#3018);
#1685=PROPERTY_DEFINITION('material property','density of part',#3018);
#1686=PROPERTY_DEFINITION('material property','material name',#3019);
#1687=PROPERTY_DEFINITION('material property','density of part',#3019);
#1688=PROPERTY_DEFINITION('material property','material name',#3020);
#1689=PROPERTY_DEFINITION('material property','density of part',#3020);
#1690=PROPERTY_DEFINITION('material property','material name',#3021);
#1691=PROPERTY_DEFINITION('material property','density of part',#3021);
#1692=PROPERTY_DEFINITION('material property','material name',#3022);
#1693=PROPERTY_DEFINITION('material property','density of part',#3022);
#1694=PROPERTY_DEFINITION('material property','material name',#3023);
#1695=PROPERTY_DEFINITION('material property','density of part',#3023);
#1696=PROPERTY_DEFINITION('material property','material name',#3024);
#1697=PROPERTY_DEFINITION('material property','density of part',#3024);
#1698=AXIS2_PLACEMENT_3D('',#2472,#1929,#1930);
#1699=AXIS2_PLACEMENT_3D('',#2473,#1931,#1932);
#1700=AXIS2_PLACEMENT_3D('',#2474,#1933,#1934);
#1701=AXIS2_PLACEMENT_3D('',#2476,#1935,#1936);
#1702=AXIS2_PLACEMENT_3D('',#2479,#1938,#1939);
#1703=AXIS2_PLACEMENT_3D('',#2480,#1940,#1941);
#1704=AXIS2_PLACEMENT_3D('',#2482,#1942,#1943);
#1705=AXIS2_PLACEMENT_3D('',#2485,#1945,#1946);
#1706=AXIS2_PLACEMENT_3D('',#2486,#1947,#1948);
#1707=AXIS2_PLACEMENT_3D('',#2488,#1949,#1950);
#1708=AXIS2_PLACEMENT_3D('',#2491,#1952,#1953);
#1709=AXIS2_PLACEMENT_3D('',#2492,#1954,#1955);
#1710=AXIS2_PLACEMENT_3D('',#2494,#1956,#1957);
#1711=AXIS2_PLACEMENT_3D('',#2497,#1959,#1960);
#1712=AXIS2_PLACEMENT_3D('',#2498,#1961,#1962);
#1713=AXIS2_PLACEMENT_3D('',#2500,#1963,#1964);
#1714=AXIS2_PLACEMENT_3D('',#2503,#1966,#1967);
#1715=AXIS2_PLACEMENT_3D('',#2504,#1968,#1969);
#1716=AXIS2_PLACEMENT_3D('',#2513,#1974,#1975);
#1717=AXIS2_PLACEMENT_3D('',#2519,#1979,#1980);
#1718=AXIS2_PLACEMENT_3D('',#2525,#1984,#1985);
#1719=AXIS2_PLACEMENT_3D('',#2528,#1988,#1989);
#1720=AXIS2_PLACEMENT_3D('',#2529,#1990,#1991);
#1721=AXIS2_PLACEMENT_3D('',#2530,#1992,#1993);
#1722=AXIS2_PLACEMENT_3D('',#2531,#1994,#1995);
#1723=AXIS2_PLACEMENT_3D('',#2533,#1996,#1997);
#1724=AXIS2_PLACEMENT_3D('',#2536,#1999,#2000);
#1725=AXIS2_PLACEMENT_3D('',#2537,#2001,#2002);
#1726=AXIS2_PLACEMENT_3D('',#2539,#2003,#2004);
#1727=AXIS2_PLACEMENT_3D('',#2542,#2006,#2007);
#1728=AXIS2_PLACEMENT_3D('',#2543,#2008,#2009);
#1729=AXIS2_PLACEMENT_3D('',#2544,#2010,#2011);
#1730=AXIS2_PLACEMENT_3D('',#2545,#2012,#2013);
#1731=AXIS2_PLACEMENT_3D('',#2546,#2014,#2015);
#1732=AXIS2_PLACEMENT_3D('',#2548,#2016,#2017);
#1733=AXIS2_PLACEMENT_3D('',#2551,#2019,#2020);
#1734=AXIS2_PLACEMENT_3D('',#2552,#2021,#2022);
#1735=AXIS2_PLACEMENT_3D('',#2554,#2023,#2024);
#1736=AXIS2_PLACEMENT_3D('',#2557,#2026,#2027);
#1737=AXIS2_PLACEMENT_3D('',#2558,#2028,#2029);
#1738=AXIS2_PLACEMENT_3D('',#2560,#2030,#2031);
#1739=AXIS2_PLACEMENT_3D('',#2563,#2033,#2034);
#1740=AXIS2_PLACEMENT_3D('',#2564,#2035,#2036);
#1741=AXIS2_PLACEMENT_3D('',#2573,#2041,#2042);
#1742=AXIS2_PLACEMENT_3D('',#2575,#2043,#2044);
#1743=AXIS2_PLACEMENT_3D('',#2577,#2045,#2046);
#1744=AXIS2_PLACEMENT_3D('',#2579,#2048,#2049);
#1745=AXIS2_PLACEMENT_3D('',#2585,#2053,#2054);
#1746=AXIS2_PLACEMENT_3D('',#2586,#2055,#2056);
#1747=AXIS2_PLACEMENT_3D('',#2587,#2057,#2058);
#1748=AXIS2_PLACEMENT_3D('',#2588,#2059,#2060);
#1749=AXIS2_PLACEMENT_3D('',#2589,#2061,#2062);
#1750=AXIS2_PLACEMENT_3D('',#2590,#2063,#2064);
#1751=AXIS2_PLACEMENT_3D('',#2591,#2065,#2066);
#1752=AXIS2_PLACEMENT_3D('',#2593,#2067,#2068);
#1753=AXIS2_PLACEMENT_3D('',#2596,#2070,#2071);
#1754=AXIS2_PLACEMENT_3D('',#2597,#2072,#2073);
#1755=AXIS2_PLACEMENT_3D('',#2599,#2074,#2075);
#1756=AXIS2_PLACEMENT_3D('',#2602,#2077,#2078);
#1757=AXIS2_PLACEMENT_3D('',#2603,#2079,#2080);
#1758=AXIS2_PLACEMENT_3D('',#2605,#2081,#2082);
#1759=AXIS2_PLACEMENT_3D('',#2608,#2084,#2085);
#1760=AXIS2_PLACEMENT_3D('',#2609,#2086,#2087);
#1761=AXIS2_PLACEMENT_3D('',#2618,#2092,#2093);
#1762=AXIS2_PLACEMENT_3D('',#2620,#2094,#2095);
#1763=AXIS2_PLACEMENT_3D('',#2622,#2096,#2097);
#1764=AXIS2_PLACEMENT_3D('',#2624,#2099,#2100);
#1765=AXIS2_PLACEMENT_3D('',#2630,#2104,#2105);
#1766=AXIS2_PLACEMENT_3D('',#2631,#2106,#2107);
#1767=AXIS2_PLACEMENT_3D('',#2632,#2108,#2109);
#1768=AXIS2_PLACEMENT_3D('',#2633,#2110,#2111);
#1769=AXIS2_PLACEMENT_3D('',#2634,#2112,#2113);
#1770=AXIS2_PLACEMENT_3D('',#2635,#2114,#2115);
#1771=AXIS2_PLACEMENT_3D('',#2636,#2116,#2117);
#1772=AXIS2_PLACEMENT_3D('',#2638,#2118,#2119);
#1773=AXIS2_PLACEMENT_3D('',#2641,#2121,#2122);
#1774=AXIS2_PLACEMENT_3D('',#2642,#2123,#2124);
#1775=AXIS2_PLACEMENT_3D('',#2644,#2125,#2126);
#1776=AXIS2_PLACEMENT_3D('',#2645,#2127,#2128);
#1777=AXIS2_PLACEMENT_3D('',#2647,#2129,#2130);
#1778=AXIS2_PLACEMENT_3D('',#2648,#2131,#2132);
#1779=AXIS2_PLACEMENT_3D('',#2650,#2133,#2134);
#1780=AXIS2_PLACEMENT_3D('',#2652,#2136,#2137);
#1781=AXIS2_PLACEMENT_3D('',#2654,#2138,#2139);
#1782=AXIS2_PLACEMENT_3D('',#2656,#2140,#2141);
#1783=AXIS2_PLACEMENT_3D('',#2657,#2142,#2143);
#1784=AXIS2_PLACEMENT_3D('',#2660,#2145,#2146);
#1785=AXIS2_PLACEMENT_3D('',#2661,#2147,#2148);
#1786=AXIS2_PLACEMENT_3D('',#2662,#2149,#2150);
#1787=AXIS2_PLACEMENT_3D('',#2664,#2152,#2153);
#1788=AXIS2_PLACEMENT_3D('',#2665,#2154,#2155);
#1789=AXIS2_PLACEMENT_3D('',#2666,#2156,#2157);
#1790=AXIS2_PLACEMENT_3D('',#2668,#2158,#2159);
#1791=AXIS2_PLACEMENT_3D('',#2671,#2161,#2162);
#1792=AXIS2_PLACEMENT_3D('',#2672,#2163,#2164);
#1793=AXIS2_PLACEMENT_3D('',#2674,#2165,#2166);
#1794=AXIS2_PLACEMENT_3D('',#2675,#2167,#2168);
#1795=AXIS2_PLACEMENT_3D('',#2677,#2169,#2170);
#1796=AXIS2_PLACEMENT_3D('',#2678,#2171,#2172);
#1797=AXIS2_PLACEMENT_3D('',#2680,#2173,#2174);
#1798=AXIS2_PLACEMENT_3D('',#2682,#2176,#2177);
#1799=AXIS2_PLACEMENT_3D('',#2684,#2178,#2179);
#1800=AXIS2_PLACEMENT_3D('',#2686,#2180,#2181);
#1801=AXIS2_PLACEMENT_3D('',#2687,#2182,#2183);
#1802=AXIS2_PLACEMENT_3D('',#2690,#2185,#2186);
#1803=AXIS2_PLACEMENT_3D('',#2691,#2187,#2188);
#1804=AXIS2_PLACEMENT_3D('',#2693,#2189,#2190);
#1805=AXIS2_PLACEMENT_3D('',#2694,#2191,#2192);
#1806=AXIS2_PLACEMENT_3D('',#2696,#2193,#2194);
#1807=AXIS2_PLACEMENT_3D('',#2698,#2196,#2197);
#1808=AXIS2_PLACEMENT_3D('',#2700,#2199,#2200);
#1809=AXIS2_PLACEMENT_3D('',#2701,#2201,#2202);
#1810=AXIS2_PLACEMENT_3D('',#2702,#2203,#2204);
#1811=AXIS2_PLACEMENT_3D('',#2704,#2205,#2206);
#1812=AXIS2_PLACEMENT_3D('',#2706,#2207,#2208);
#1813=AXIS2_PLACEMENT_3D('',#2707,#2209,#2210);
#1814=AXIS2_PLACEMENT_3D('',#2709,#2211,#2212);
#1815=AXIS2_PLACEMENT_3D('',#2711,#2214,#2215);
#1816=AXIS2_PLACEMENT_3D('',#2713,#2216,#2217);
#1817=AXIS2_PLACEMENT_3D('',#2714,#2218,#2219);
#1818=AXIS2_PLACEMENT_3D('',#2717,#2221,#2222);
#1819=AXIS2_PLACEMENT_3D('',#2718,#2223,#2224);
#1820=AXIS2_PLACEMENT_3D('',#2721,#2226,#2227);
#1821=AXIS2_PLACEMENT_3D('',#2722,#2228,#2229);
#1822=AXIS2_PLACEMENT_3D('',#2723,#2230,#2231);
#1823=AXIS2_PLACEMENT_3D('',#2724,#2232,#2233);
#1824=AXIS2_PLACEMENT_3D('',#2726,#2234,#2235);
#1825=AXIS2_PLACEMENT_3D('',#2729,#2237,#2238);
#1826=AXIS2_PLACEMENT_3D('',#2730,#2239,#2240);
#1827=AXIS2_PLACEMENT_3D('',#2732,#2241,#2242);
#1828=AXIS2_PLACEMENT_3D('',#2735,#2244,#2245);
#1829=AXIS2_PLACEMENT_3D('',#2736,#2246,#2247);
#1830=AXIS2_PLACEMENT_3D('',#2745,#2252,#2253);
#1831=AXIS2_PLACEMENT_3D('',#2747,#2254,#2255);
#1832=AXIS2_PLACEMENT_3D('',#2749,#2256,#2257);
#1833=AXIS2_PLACEMENT_3D('',#2751,#2259,#2260);
#1834=AXIS2_PLACEMENT_3D('',#2757,#2264,#2265);
#1835=AXIS2_PLACEMENT_3D('',#2758,#2266,#2267);
#1836=AXIS2_PLACEMENT_3D('',#2759,#2268,#2269);
#1837=AXIS2_PLACEMENT_3D('',#2760,#2270,#2271);
#1838=AXIS2_PLACEMENT_3D('',#2761,#2272,#2273);
#1839=AXIS2_PLACEMENT_3D('',#2762,#2274,#2275);
#1840=AXIS2_PLACEMENT_3D('',#2763,#2276,#2277);
#1841=AXIS2_PLACEMENT_3D('',#2765,#2278,#2279);
#1842=AXIS2_PLACEMENT_3D('',#2768,#2281,#2282);
#1843=AXIS2_PLACEMENT_3D('',#2769,#2283,#2284);
#1844=AXIS2_PLACEMENT_3D('',#2771,#2285,#2286);
#1845=AXIS2_PLACEMENT_3D('',#2774,#2288,#2289);
#1846=AXIS2_PLACEMENT_3D('',#2775,#2290,#2291);
#1847=AXIS2_PLACEMENT_3D('',#2776,#2292,#2293);
#1848=AXIS2_PLACEMENT_3D('',#2777,#2294,#2295);
#1849=AXIS2_PLACEMENT_3D('',#2778,#2296,#2297);
#1850=AXIS2_PLACEMENT_3D('',#2780,#2298,#2299);
#1851=AXIS2_PLACEMENT_3D('',#2783,#2301,#2302);
#1852=AXIS2_PLACEMENT_3D('',#2784,#2303,#2304);
#1853=AXIS2_PLACEMENT_3D('',#2786,#2305,#2306);
#1854=AXIS2_PLACEMENT_3D('',#2787,#2307,#2308);
#1855=AXIS2_PLACEMENT_3D('',#2789,#2309,#2310);
#1856=AXIS2_PLACEMENT_3D('',#2790,#2311,#2312);
#1857=AXIS2_PLACEMENT_3D('',#2792,#2313,#2314);
#1858=AXIS2_PLACEMENT_3D('',#2794,#2316,#2317);
#1859=AXIS2_PLACEMENT_3D('',#2796,#2318,#2319);
#1860=AXIS2_PLACEMENT_3D('',#2798,#2320,#2321);
#1861=AXIS2_PLACEMENT_3D('',#2799,#2322,#2323);
#1862=AXIS2_PLACEMENT_3D('',#2802,#2325,#2326);
#1863=AXIS2_PLACEMENT_3D('',#2803,#2327,#2328);
#1864=AXIS2_PLACEMENT_3D('',#2804,#2329,#2330);
#1865=AXIS2_PLACEMENT_3D('',#2806,#2332,#2333);
#1866=AXIS2_PLACEMENT_3D('',#2807,#2334,#2335);
#1867=AXIS2_PLACEMENT_3D('',#2808,#2336,#2337);
#1868=AXIS2_PLACEMENT_3D('',#2810,#2338,#2339);
#1869=AXIS2_PLACEMENT_3D('',#2813,#2341,#2342);
#1870=AXIS2_PLACEMENT_3D('',#2814,#2343,#2344);
#1871=AXIS2_PLACEMENT_3D('',#2816,#2345,#2346);
#1872=AXIS2_PLACEMENT_3D('',#2819,#2348,#2349);
#1873=AXIS2_PLACEMENT_3D('',#2820,#2350,#2351);
#1874=AXIS2_PLACEMENT_3D('',#2821,#2352,#2353);
#1875=AXIS2_PLACEMENT_3D('',#2822,#2354,#2355);
#1876=AXIS2_PLACEMENT_3D('',#2823,#2356,#2357);
#1877=AXIS2_PLACEMENT_3D('',#2832,#2362,#2363);
#1878=AXIS2_PLACEMENT_3D('',#2841,#2368,#2369);
#1879=AXIS2_PLACEMENT_3D('',#2842,#2370,#2371);
#1880=AXIS2_PLACEMENT_3D('',#2843,#2372,#2373);
#1881=AXIS2_PLACEMENT_3D('',#2844,#2374,#2375);
#1882=AXIS2_PLACEMENT_3D('',#2845,#2376,#2377);
#1883=AXIS2_PLACEMENT_3D('',#2846,#2378,#2379);
#1884=AXIS2_PLACEMENT_3D('',#2847,#2380,#2381);
#1885=AXIS2_PLACEMENT_3D('',#2848,#2382,#2383);
#1886=AXIS2_PLACEMENT_3D('',#2849,#2384,#2385);
#1887=AXIS2_PLACEMENT_3D('',#2850,#2386,#2387);
#1888=AXIS2_PLACEMENT_3D('',#2852,#2388,#2389);
#1889=AXIS2_PLACEMENT_3D('',#2855,#2391,#2392);
#1890=AXIS2_PLACEMENT_3D('',#2856,#2393,#2394);
#1891=AXIS2_PLACEMENT_3D('',#2857,#2395,#2396);
#1892=AXIS2_PLACEMENT_3D('',#2860,#2398,#2399);
#1893=AXIS2_PLACEMENT_3D('',#2861,#2400,#2401);
#1894=AXIS2_PLACEMENT_3D('',#2862,#2402,#2403);
#1895=AXIS2_PLACEMENT_3D('',#2863,#2404,#2405);
#1896=AXIS2_PLACEMENT_3D('',#2864,#2406,#2407);
#1897=AXIS2_PLACEMENT_3D('',#2865,#2408,#2409);
#1898=AXIS2_PLACEMENT_3D('',#2866,#2410,#2411);
#1899=AXIS2_PLACEMENT_3D('',#2867,#2412,#2413);
#1900=AXIS2_PLACEMENT_3D('',#2868,#2414,#2415);
#1901=AXIS2_PLACEMENT_3D('',#2869,#2416,#2417);
#1902=AXIS2_PLACEMENT_3D('',#2870,#2418,#2419);
#1903=AXIS2_PLACEMENT_3D('',#2871,#2420,#2421);
#1904=AXIS2_PLACEMENT_3D('',#2872,#2422,#2423);
#1905=AXIS2_PLACEMENT_3D('',#2873,#2424,#2425);
#1906=AXIS2_PLACEMENT_3D('',#2874,#2426,#2427);
#1907=AXIS2_PLACEMENT_3D('',#2875,#2428,#2429);
#1908=AXIS2_PLACEMENT_3D('',#2876,#2430,#2431);
#1909=AXIS2_PLACEMENT_3D('',#2877,#2432,#2433);
#1910=AXIS2_PLACEMENT_3D('',#2878,#2434,#2435);
#1911=AXIS2_PLACEMENT_3D('',#2879,#2436,#2437);
#1912=AXIS2_PLACEMENT_3D('',#2880,#2438,#2439);
#1913=AXIS2_PLACEMENT_3D('',#2881,#2440,#2441);
#1914=AXIS2_PLACEMENT_3D('',#2882,#2442,#2443);
#1915=AXIS2_PLACEMENT_3D('',#2883,#2444,#2445);
#1916=AXIS2_PLACEMENT_3D('',#2884,#2446,#2447);
#1917=AXIS2_PLACEMENT_3D('',#2885,#2448,#2449);
#1918=AXIS2_PLACEMENT_3D('',#2886,#2450,#2451);
#1919=AXIS2_PLACEMENT_3D('',#2887,#2452,#2453);
#1920=AXIS2_PLACEMENT_3D('',#2888,#2454,#2455);
#1921=AXIS2_PLACEMENT_3D('',#2889,#2456,#2457);
#1922=AXIS2_PLACEMENT_3D('',#2890,#2458,#2459);
#1923=AXIS2_PLACEMENT_3D('',#2891,#2460,#2461);
#1924=AXIS2_PLACEMENT_3D('',#2892,#2462,#2463);
#1925=AXIS2_PLACEMENT_3D('',#2893,#2464,#2465);
#1926=AXIS2_PLACEMENT_3D('',#2894,#2466,#2467);
#1927=AXIS2_PLACEMENT_3D('',#2895,#2468,#2469);
#1928=AXIS2_PLACEMENT_3D('',#2896,#2470,#2471);
#1929=DIRECTION('axis',(0.,0.,1.));
#1930=DIRECTION('refdir',(1.,0.,0.));
#1931=DIRECTION('axis',(0.,0.,1.));
#1932=DIRECTION('refdir',(1.,0.,0.));
#1933=DIRECTION('center_axis',(0.,0.,-1.));
#1934=DIRECTION('ref_axis',(1.,0.,0.));
#1935=DIRECTION('center_axis',(0.,0.,-1.));
#1936=DIRECTION('ref_axis',(1.,0.,0.));
#1937=DIRECTION('',(0.,0.,-1.));
#1938=DIRECTION('center_axis',(0.,0.,1.));
#1939=DIRECTION('ref_axis',(1.,0.,0.));
#1940=DIRECTION('center_axis',(0.,0.,-1.));
#1941=DIRECTION('ref_axis',(1.,0.,0.));
#1942=DIRECTION('center_axis',(0.,0.,-1.));
#1943=DIRECTION('ref_axis',(1.,0.,0.));
#1944=DIRECTION('',(0.,0.,-1.));
#1945=DIRECTION('center_axis',(0.,0.,1.));
#1946=DIRECTION('ref_axis',(1.,0.,0.));
#1947=DIRECTION('center_axis',(0.,0.,-1.));
#1948=DIRECTION('ref_axis',(1.,0.,0.));
#1949=DIRECTION('center_axis',(0.,0.,-1.));
#1950=DIRECTION('ref_axis',(1.,0.,0.));
#1951=DIRECTION('',(0.,0.,-1.));
#1952=DIRECTION('center_axis',(0.,0.,1.));
#1953=DIRECTION('ref_axis',(1.,0.,0.));
#1954=DIRECTION('center_axis',(0.,0.,-1.));
#1955=DIRECTION('ref_axis',(1.,0.,0.));
#1956=DIRECTION('center_axis',(0.,0.,-1.));
#1957=DIRECTION('ref_axis',(1.,0.,0.));
#1958=DIRECTION('',(0.,0.,-1.));
#1959=DIRECTION('center_axis',(0.,0.,1.));
#1960=DIRECTION('ref_axis',(1.,0.,0.));
#1961=DIRECTION('center_axis',(0.,0.,-1.));
#1962=DIRECTION('ref_axis',(1.,0.,0.));
#1963=DIRECTION('center_axis',(0.,0.,-1.));
#1964=DIRECTION('ref_axis',(1.,0.,0.));
#1965=DIRECTION('',(0.,0.,-1.));
#1966=DIRECTION('center_axis',(0.,0.,1.));
#1967=DIRECTION('ref_axis',(1.,0.,0.));
#1968=DIRECTION('center_axis',(0.,1.,0.));
#1969=DIRECTION('ref_axis',(-1.,0.,0.));
#1970=DIRECTION('',(-1.,0.,0.));
#1971=DIRECTION('',(0.,0.,1.));
#1972=DIRECTION('',(-1.,0.,0.));
#1973=DIRECTION('',(0.,0.,1.));
#1974=DIRECTION('center_axis',(1.,0.,0.));
#1975=DIRECTION('ref_axis',(0.,1.,0.));
#1976=DIRECTION('',(0.,1.,0.));
#1977=DIRECTION('',(0.,1.,0.));
#1978=DIRECTION('',(0.,0.,1.));
#1979=DIRECTION('center_axis',(0.,-1.,0.));
#1980=DIRECTION('ref_axis',(1.,0.,0.));
#1981=DIRECTION('',(1.,0.,0.));
#1982=DIRECTION('',(1.,0.,0.));
#1983=DIRECTION('',(0.,0.,1.));
#1984=DIRECTION('center_axis',(-1.,0.,0.));
#1985=DIRECTION('ref_axis',(0.,-1.,0.));
#1986=DIRECTION('',(0.,-1.,0.));
#1987=DIRECTION('',(0.,-1.,0.));
#1988=DIRECTION('center_axis',(0.,0.,1.));
#1989=DIRECTION('ref_axis',(1.,0.,0.));
#1990=DIRECTION('center_axis',(0.,0.,1.));
#1991=DIRECTION('ref_axis',(1.,0.,0.));
#1992=DIRECTION('axis',(0.,0.,1.));
#1993=DIRECTION('refdir',(1.,0.,0.));
#1994=DIRECTION('center_axis',(0.,0.,1.));
#1995=DIRECTION('ref_axis',(1.,0.,0.));
#1996=DIRECTION('center_axis',(0.,0.,-1.));
#1997=DIRECTION('ref_axis',(1.,0.,0.));
#1998=DIRECTION('',(0.,0.,-1.));
#1999=DIRECTION('center_axis',(0.,0.,-1.));
#2000=DIRECTION('ref_axis',(1.,0.,0.));
#2001=DIRECTION('center_axis',(0.,0.,1.));
#2002=DIRECTION('ref_axis',(1.,0.,0.));
#2003=DIRECTION('center_axis',(0.,0.,1.));
#2004=DIRECTION('ref_axis',(1.,0.,0.));
#2005=DIRECTION('',(0.,0.,-1.));
#2006=DIRECTION('center_axis',(0.,0.,1.));
#2007=DIRECTION('ref_axis',(1.,0.,0.));
#2008=DIRECTION('center_axis',(0.,0.,1.));
#2009=DIRECTION('ref_axis',(1.,0.,0.));
#2010=DIRECTION('center_axis',(0.,0.,1.));
#2011=DIRECTION('ref_axis',(1.,0.,0.));
#2012=DIRECTION('axis',(0.,0.,1.));
#2013=DIRECTION('refdir',(1.,0.,0.));
#2014=DIRECTION('center_axis',(0.,0.,-1.));
#2015=DIRECTION('ref_axis',(1.,0.,0.));
#2016=DIRECTION('center_axis',(0.,0.,-1.));
#2017=DIRECTION('ref_axis',(1.,0.,0.));
#2018=DIRECTION('',(0.,0.,-1.));
#2019=DIRECTION('center_axis',(0.,0.,1.));
#2020=DIRECTION('ref_axis',(1.,0.,0.));
#2021=DIRECTION('center_axis',(0.,0.,-1.));
#2022=DIRECTION('ref_axis',(1.,0.,0.));
#2023=DIRECTION('center_axis',(0.,0.,-1.));
#2024=DIRECTION('ref_axis',(1.,0.,0.));
#2025=DIRECTION('',(0.,0.,-1.));
#2026=DIRECTION('center_axis',(0.,0.,1.));
#2027=DIRECTION('ref_axis',(1.,0.,0.));
#2028=DIRECTION('center_axis',(0.,0.,-1.));
#2029=DIRECTION('ref_axis',(1.,0.,0.));
#2030=DIRECTION('center_axis',(0.,0.,-1.));
#2031=DIRECTION('ref_axis',(1.,0.,0.));
#2032=DIRECTION('',(0.,0.,-1.));
#2033=DIRECTION('center_axis',(0.,0.,1.));
#2034=DIRECTION('ref_axis',(1.,0.,0.));
#2035=DIRECTION('center_axis',(0.,1.,0.));
#2036=DIRECTION('ref_axis',(-1.,0.,0.));
#2037=DIRECTION('',(-1.,0.,0.));
#2038=DIRECTION('',(0.,0.,1.));
#2039=DIRECTION('',(-1.,0.,0.));
#2040=DIRECTION('',(0.,0.,1.));
#2041=DIRECTION('center_axis',(0.,0.,1.));
#2042=DIRECTION('ref_axis',(0.,-1.,0.));
#2043=DIRECTION('center_axis',(0.,0.,1.));
#2044=DIRECTION('ref_axis',(0.,-1.,0.));
#2045=DIRECTION('center_axis',(0.,0.,1.));
#2046=DIRECTION('ref_axis',(0.,-1.,0.));
#2047=DIRECTION('',(0.,0.,1.));
#2048=DIRECTION('center_axis',(0.,-1.,0.));
#2049=DIRECTION('ref_axis',(1.,0.,0.));
#2050=DIRECTION('',(1.,0.,0.));
#2051=DIRECTION('',(1.,0.,0.));
#2052=DIRECTION('',(0.,0.,1.));
#2053=DIRECTION('center_axis',(0.,0.,1.));
#2054=DIRECTION('ref_axis',(0.,1.,0.));
#2055=DIRECTION('center_axis',(0.,0.,1.));
#2056=DIRECTION('ref_axis',(0.,1.,0.));
#2057=DIRECTION('center_axis',(0.,0.,1.));
#2058=DIRECTION('ref_axis',(0.,1.,0.));
#2059=DIRECTION('center_axis',(0.,0.,1.));
#2060=DIRECTION('ref_axis',(1.,0.,0.));
#2061=DIRECTION('center_axis',(0.,0.,1.));
#2062=DIRECTION('ref_axis',(1.,0.,0.));
#2063=DIRECTION('axis',(0.,0.,1.));
#2064=DIRECTION('refdir',(1.,0.,0.));
#2065=DIRECTION('center_axis',(0.,0.,-1.));
#2066=DIRECTION('ref_axis',(1.,0.,0.));
#2067=DIRECTION('center_axis',(0.,0.,-1.));
#2068=DIRECTION('ref_axis',(1.,0.,0.));
#2069=DIRECTION('',(0.,0.,-1.));
#2070=DIRECTION('center_axis',(0.,0.,1.));
#2071=DIRECTION('ref_axis',(1.,0.,0.));
#2072=DIRECTION('center_axis',(0.,0.,-1.));
#2073=DIRECTION('ref_axis',(1.,0.,0.));
#2074=DIRECTION('center_axis',(0.,0.,-1.));
#2075=DIRECTION('ref_axis',(1.,0.,0.));
#2076=DIRECTION('',(0.,0.,-1.));
#2077=DIRECTION('center_axis',(0.,0.,1.));
#2078=DIRECTION('ref_axis',(1.,0.,0.));
#2079=DIRECTION('center_axis',(0.,0.,-1.));
#2080=DIRECTION('ref_axis',(1.,0.,0.));
#2081=DIRECTION('center_axis',(0.,0.,-1.));
#2082=DIRECTION('ref_axis',(1.,0.,0.));
#2083=DIRECTION('',(0.,0.,-1.));
#2084=DIRECTION('center_axis',(0.,0.,1.));
#2085=DIRECTION('ref_axis',(1.,0.,0.));
#2086=DIRECTION('center_axis',(0.,1.,0.));
#2087=DIRECTION('ref_axis',(-1.,0.,0.));
#2088=DIRECTION('',(-1.,0.,0.));
#2089=DIRECTION('',(0.,0.,1.));
#2090=DIRECTION('',(-1.,0.,0.));
#2091=DIRECTION('',(0.,0.,1.));
#2092=DIRECTION('center_axis',(0.,0.,1.));
#2093=DIRECTION('ref_axis',(0.,-1.,0.));
#2094=DIRECTION('center_axis',(0.,0.,1.));
#2095=DIRECTION('ref_axis',(0.,-1.,0.));
#2096=DIRECTION('center_axis',(0.,0.,1.));
#2097=DIRECTION('ref_axis',(0.,-1.,0.));
#2098=DIRECTION('',(0.,0.,1.));
#2099=DIRECTION('center_axis',(0.,-1.,0.));
#2100=DIRECTION('ref_axis',(1.,0.,0.));
#2101=DIRECTION('',(1.,0.,0.));
#2102=DIRECTION('',(1.,0.,0.));
#2103=DIRECTION('',(0.,0.,1.));
#2104=DIRECTION('center_axis',(0.,0.,1.));
#2105=DIRECTION('ref_axis',(0.,1.,0.));
#2106=DIRECTION('center_axis',(0.,0.,1.));
#2107=DIRECTION('ref_axis',(0.,1.,0.));
#2108=DIRECTION('center_axis',(0.,0.,1.));
#2109=DIRECTION('ref_axis',(0.,1.,0.));
#2110=DIRECTION('center_axis',(0.,0.,1.));
#2111=DIRECTION('ref_axis',(1.,0.,0.));
#2112=DIRECTION('center_axis',(0.,0.,1.));
#2113=DIRECTION('ref_axis',(1.,0.,0.));
#2114=DIRECTION('axis',(0.,0.,1.));
#2115=DIRECTION('refdir',(1.,0.,0.));
#2116=DIRECTION('center_axis',(0.,0.,1.));
#2117=DIRECTION('ref_axis',(1.,0.,0.));
#2118=DIRECTION('center_axis',(0.,0.,1.));
#2119=DIRECTION('ref_axis',(1.,0.,0.));
#2120=DIRECTION('',(0.,0.,1.));
#2121=DIRECTION('center_axis',(0.,0.,1.));
#2122=DIRECTION('ref_axis',(1.,0.,0.));
#2123=DIRECTION('center_axis',(0.,0.,-1.));
#2124=DIRECTION('ref_axis',(-1.,0.,0.));
#2125=DIRECTION('center_axis',(0.,0.,-1.));
#2126=DIRECTION('ref_axis',(1.,0.,0.));
#2127=DIRECTION('center_axis',(0.,0.,1.));
#2128=DIRECTION('ref_axis',(1.,0.,0.));
#2129=DIRECTION('center_axis',(0.,0.,1.));
#2130=DIRECTION('ref_axis',(1.,0.,0.));
#2131=DIRECTION('center_axis',(0.,0.,1.));
#2132=DIRECTION('ref_axis',(1.,0.,0.));
#2133=DIRECTION('center_axis',(0.,0.,1.));
#2134=DIRECTION('ref_axis',(1.,0.,0.));
#2135=DIRECTION('',(0.,0.,-1.));
#2136=DIRECTION('center_axis',(0.,0.,1.));
#2137=DIRECTION('ref_axis',(1.,0.,0.));
#2138=DIRECTION('center_axis',(0.,0.,1.));
#2139=DIRECTION('ref_axis',(1.,0.,0.));
#2140=DIRECTION('center_axis',(0.,0.,1.));
#2141=DIRECTION('ref_axis',(1.,0.,0.));
#2142=DIRECTION('center_axis',(0.,0.,1.));
#2143=DIRECTION('ref_axis',(1.,0.,0.));
#2144=DIRECTION('',(0.,0.,-1.));
#2145=DIRECTION('center_axis',(0.,0.,1.));
#2146=DIRECTION('ref_axis',(1.,0.,0.));
#2147=DIRECTION('center_axis',(0.,0.,1.));
#2148=DIRECTION('ref_axis',(1.,0.,0.));
#2149=DIRECTION('center_axis',(0.,0.,1.));
#2150=DIRECTION('ref_axis',(1.,0.,0.));
#2151=DIRECTION('',(0.,0.,-1.));
#2152=DIRECTION('center_axis',(0.,0.,1.));
#2153=DIRECTION('ref_axis',(1.,0.,0.));
#2154=DIRECTION('axis',(0.,0.,1.));
#2155=DIRECTION('refdir',(1.,0.,0.));
#2156=DIRECTION('center_axis',(0.,0.,1.));
#2157=DIRECTION('ref_axis',(1.,0.,0.));
#2158=DIRECTION('center_axis',(0.,0.,1.));
#2159=DIRECTION('ref_axis',(1.,0.,0.));
#2160=DIRECTION('',(0.,0.,1.));
#2161=DIRECTION('center_axis',(0.,0.,1.));
#2162=DIRECTION('ref_axis',(1.,0.,0.));
#2163=DIRECTION('center_axis',(0.,0.,-1.));
#2164=DIRECTION('ref_axis',(-1.,0.,0.));
#2165=DIRECTION('center_axis',(0.,0.,-1.));
#2166=DIRECTION('ref_axis',(1.,0.,0.));
#2167=DIRECTION('center_axis',(0.,0.,1.));
#2168=DIRECTION('ref_axis',(1.,0.,0.));
#2169=DIRECTION('center_axis',(0.,0.,1.));
#2170=DIRECTION('ref_axis',(1.,0.,0.));
#2171=DIRECTION('center_axis',(0.,0.,1.));
#2172=DIRECTION('ref_axis',(1.,0.,0.));
#2173=DIRECTION('center_axis',(0.,0.,1.));
#2174=DIRECTION('ref_axis',(1.,0.,0.));
#2175=DIRECTION('',(0.,0.,-1.));
#2176=DIRECTION('center_axis',(0.,0.,1.));
#2177=DIRECTION('ref_axis',(1.,0.,0.));
#2178=DIRECTION('center_axis',(0.,0.,1.));
#2179=DIRECTION('ref_axis',(1.,0.,0.));
#2180=DIRECTION('center_axis',(0.,0.,1.));
#2181=DIRECTION('ref_axis',(1.,0.,0.));
#2182=DIRECTION('center_axis',(0.,0.,1.));
#2183=DIRECTION('ref_axis',(1.,0.,0.));
#2184=DIRECTION('',(0.,0.,-1.));
#2185=DIRECTION('center_axis',(0.,0.,1.));
#2186=DIRECTION('ref_axis',(1.,0.,0.));
#2187=DIRECTION('center_axis',(0.,0.,1.));
#2188=DIRECTION('ref_axis',(1.,0.,0.));
#2189=DIRECTION('center_axis',(0.,0.,-1.));
#2190=DIRECTION('ref_axis',(1.,0.,0.));
#2191=DIRECTION('center_axis',(0.,0.,1.));
#2192=DIRECTION('ref_axis',(1.,0.,0.));
#2193=DIRECTION('center_axis',(0.,0.,-1.));
#2194=DIRECTION('ref_axis',(1.,0.,0.));
#2195=DIRECTION('',(0.,0.,-1.));
#2196=DIRECTION('center_axis',(0.,0.,1.));
#2197=DIRECTION('ref_axis',(1.,0.,0.));
#2198=DIRECTION('',(0.,0.,-1.));
#2199=DIRECTION('center_axis',(0.,0.,1.));
#2200=DIRECTION('ref_axis',(1.,0.,0.));
#2201=DIRECTION('axis',(0.,0.,1.));
#2202=DIRECTION('refdir',(1.,0.,0.));
#2203=DIRECTION('center_axis',(0.,0.,1.));
#2204=DIRECTION('ref_axis',(1.,0.,0.));
#2205=DIRECTION('center_axis',(0.,0.,1.));
#2206=DIRECTION('ref_axis',(1.,0.,0.));
#2207=DIRECTION('center_axis',(0.,0.,1.));
#2208=DIRECTION('ref_axis',(1.,0.,0.));
#2209=DIRECTION('center_axis',(0.,0.,1.));
#2210=DIRECTION('ref_axis',(1.,0.,0.));
#2211=DIRECTION('center_axis',(0.,0.,1.));
#2212=DIRECTION('ref_axis',(1.,0.,0.));
#2213=DIRECTION('',(0.,0.,-1.));
#2214=DIRECTION('center_axis',(0.,0.,1.));
#2215=DIRECTION('ref_axis',(1.,0.,0.));
#2216=DIRECTION('center_axis',(0.,0.,-1.));
#2217=DIRECTION('ref_axis',(1.,0.,0.));
#2218=DIRECTION('center_axis',(0.,0.,1.));
#2219=DIRECTION('ref_axis',(1.,0.,0.));
#2220=DIRECTION('',(0.,0.,-1.));
#2221=DIRECTION('center_axis',(0.,0.,-1.));
#2222=DIRECTION('ref_axis',(1.,0.,0.));
#2223=DIRECTION('center_axis',(0.,0.,1.));
#2224=DIRECTION('ref_axis',(1.,0.,0.));
#2225=DIRECTION('',(0.,0.,-1.));
#2226=DIRECTION('center_axis',(0.,0.,1.));
#2227=DIRECTION('ref_axis',(1.,0.,0.));
#2228=DIRECTION('center_axis',(0.,0.,1.));
#2229=DIRECTION('ref_axis',(1.,0.,0.));
#2230=DIRECTION('axis',(0.,0.,1.));
#2231=DIRECTION('refdir',(1.,0.,0.));
#2232=DIRECTION('center_axis',(0.,0.,-1.));
#2233=DIRECTION('ref_axis',(1.,0.,0.));
#2234=DIRECTION('center_axis',(0.,0.,-1.));
#2235=DIRECTION('ref_axis',(1.,0.,0.));
#2236=DIRECTION('',(0.,0.,-1.));
#2237=DIRECTION('center_axis',(0.,0.,1.));
#2238=DIRECTION('ref_axis',(1.,0.,0.));
#2239=DIRECTION('center_axis',(0.,0.,-1.));
#2240=DIRECTION('ref_axis',(1.,0.,0.));
#2241=DIRECTION('center_axis',(0.,0.,-1.));
#2242=DIRECTION('ref_axis',(1.,0.,0.));
#2243=DIRECTION('',(0.,0.,-1.));
#2244=DIRECTION('center_axis',(0.,0.,1.));
#2245=DIRECTION('ref_axis',(1.,0.,0.));
#2246=DIRECTION('center_axis',(0.,1.,0.));
#2247=DIRECTION('ref_axis',(-1.,0.,0.));
#2248=DIRECTION('',(-1.,0.,0.));
#2249=DIRECTION('',(0.,0.,1.));
#2250=DIRECTION('',(-1.,0.,0.));
#2251=DIRECTION('',(0.,0.,1.));
#2252=DIRECTION('center_axis',(0.,0.,1.));
#2253=DIRECTION('ref_axis',(0.,-1.,0.));
#2254=DIRECTION('center_axis',(0.,0.,1.));
#2255=DIRECTION('ref_axis',(0.,-1.,0.));
#2256=DIRECTION('center_axis',(0.,0.,1.));
#2257=DIRECTION('ref_axis',(0.,-1.,0.));
#2258=DIRECTION('',(0.,0.,1.));
#2259=DIRECTION('center_axis',(0.,-1.,0.));
#2260=DIRECTION('ref_axis',(1.,0.,0.));
#2261=DIRECTION('',(1.,0.,0.));
#2262=DIRECTION('',(1.,0.,0.));
#2263=DIRECTION('',(0.,0.,1.));
#2264=DIRECTION('center_axis',(0.,0.,1.));
#2265=DIRECTION('ref_axis',(0.,1.,0.));
#2266=DIRECTION('center_axis',(0.,0.,1.));
#2267=DIRECTION('ref_axis',(0.,1.,0.));
#2268=DIRECTION('center_axis',(0.,0.,1.));
#2269=DIRECTION('ref_axis',(0.,1.,0.));
#2270=DIRECTION('center_axis',(0.,0.,1.));
#2271=DIRECTION('ref_axis',(1.,0.,0.));
#2272=DIRECTION('center_axis',(0.,0.,1.));
#2273=DIRECTION('ref_axis',(1.,0.,0.));
#2274=DIRECTION('axis',(0.,0.,1.));
#2275=DIRECTION('refdir',(1.,0.,0.));
#2276=DIRECTION('center_axis',(0.,0.,1.));
#2277=DIRECTION('ref_axis',(1.,0.,0.));
#2278=DIRECTION('center_axis',(0.,0.,-1.));
#2279=DIRECTION('ref_axis',(1.,0.,0.));
#2280=DIRECTION('',(0.,0.,-1.));
#2281=DIRECTION('center_axis',(0.,0.,-1.));
#2282=DIRECTION('ref_axis',(1.,0.,0.));
#2283=DIRECTION('center_axis',(0.,0.,1.));
#2284=DIRECTION('ref_axis',(1.,0.,0.));
#2285=DIRECTION('center_axis',(0.,0.,1.));
#2286=DIRECTION('ref_axis',(1.,0.,0.));
#2287=DIRECTION('',(0.,0.,-1.));
#2288=DIRECTION('center_axis',(0.,0.,1.));
#2289=DIRECTION('ref_axis',(1.,0.,0.));
#2290=DIRECTION('center_axis',(0.,0.,1.));
#2291=DIRECTION('ref_axis',(1.,0.,0.));
#2292=DIRECTION('center_axis',(0.,0.,1.));
#2293=DIRECTION('ref_axis',(1.,0.,0.));
#2294=DIRECTION('axis',(0.,0.,1.));
#2295=DIRECTION('refdir',(1.,0.,0.));
#2296=DIRECTION('center_axis',(0.,0.,1.));
#2297=DIRECTION('ref_axis',(1.,0.,0.));
#2298=DIRECTION('center_axis',(0.,0.,1.));
#2299=DIRECTION('ref_axis',(1.,0.,0.));
#2300=DIRECTION('',(0.,0.,1.));
#2301=DIRECTION('center_axis',(0.,0.,1.));
#2302=DIRECTION('ref_axis',(1.,0.,0.));
#2303=DIRECTION('center_axis',(0.,0.,-1.));
#2304=DIRECTION('ref_axis',(-1.,0.,0.));
#2305=DIRECTION('center_axis',(0.,0.,-1.));
#2306=DIRECTION('ref_axis',(1.,0.,0.));
#2307=DIRECTION('center_axis',(0.,0.,1.));
#2308=DIRECTION('ref_axis',(1.,0.,0.));
#2309=DIRECTION('center_axis',(0.,0.,1.));
#2310=DIRECTION('ref_axis',(1.,0.,0.));
#2311=DIRECTION('center_axis',(0.,0.,1.));
#2312=DIRECTION('ref_axis',(1.,0.,0.));
#2313=DIRECTION('center_axis',(0.,0.,1.));
#2314=DIRECTION('ref_axis',(1.,0.,0.));
#2315=DIRECTION('',(0.,0.,-1.));
#2316=DIRECTION('center_axis',(0.,0.,1.));
#2317=DIRECTION('ref_axis',(1.,0.,0.));
#2318=DIRECTION('center_axis',(0.,0.,1.));
#2319=DIRECTION('ref_axis',(1.,0.,0.));
#2320=DIRECTION('center_axis',(0.,0.,1.));
#2321=DIRECTION('ref_axis',(1.,0.,0.));
#2322=DIRECTION('center_axis',(0.,0.,1.));
#2323=DIRECTION('ref_axis',(1.,0.,0.));
#2324=DIRECTION('',(0.,0.,-1.));
#2325=DIRECTION('center_axis',(0.,0.,1.));
#2326=DIRECTION('ref_axis',(1.,0.,0.));
#2327=DIRECTION('center_axis',(0.,0.,1.));
#2328=DIRECTION('ref_axis',(1.,0.,0.));
#2329=DIRECTION('center_axis',(0.,0.,1.));
#2330=DIRECTION('ref_axis',(1.,0.,0.));
#2331=DIRECTION('',(0.,0.,-1.));
#2332=DIRECTION('center_axis',(0.,0.,1.));
#2333=DIRECTION('ref_axis',(1.,0.,0.));
#2334=DIRECTION('axis',(0.,0.,1.));
#2335=DIRECTION('refdir',(1.,0.,0.));
#2336=DIRECTION('center_axis',(0.,0.,1.));
#2337=DIRECTION('ref_axis',(1.,0.,0.));
#2338=DIRECTION('center_axis',(0.,0.,-1.));
#2339=DIRECTION('ref_axis',(1.,0.,0.));
#2340=DIRECTION('',(0.,0.,-1.));
#2341=DIRECTION('center_axis',(0.,0.,-1.));
#2342=DIRECTION('ref_axis',(1.,0.,0.));
#2343=DIRECTION('center_axis',(0.,0.,1.));
#2344=DIRECTION('ref_axis',(1.,0.,0.));
#2345=DIRECTION('center_axis',(0.,0.,1.));
#2346=DIRECTION('ref_axis',(1.,0.,0.));
#2347=DIRECTION('',(0.,0.,-1.));
#2348=DIRECTION('center_axis',(0.,0.,1.));
#2349=DIRECTION('ref_axis',(1.,0.,0.));
#2350=DIRECTION('center_axis',(0.,0.,1.));
#2351=DIRECTION('ref_axis',(1.,0.,0.));
#2352=DIRECTION('center_axis',(0.,0.,1.));
#2353=DIRECTION('ref_axis',(1.,0.,0.));
#2354=DIRECTION('axis',(0.,0.,1.));
#2355=DIRECTION('refdir',(1.,0.,0.));
#2356=DIRECTION('center_axis',(-1.,0.,0.));
#2357=DIRECTION('ref_axis',(0.,1.,0.));
#2358=DIRECTION('',(0.,0.,1.));
#2359=DIRECTION('',(0.,-1.,0.));
#2360=DIRECTION('',(0.,0.,-1.));
#2361=DIRECTION('',(0.,1.,0.));
#2362=DIRECTION('center_axis',(1.,0.,0.));
#2363=DIRECTION('ref_axis',(0.,-1.,0.));
#2364=DIRECTION('',(0.,0.,-1.));
#2365=DIRECTION('',(0.,-1.,0.));
#2366=DIRECTION('',(0.,0.,1.));
#2367=DIRECTION('',(0.,1.,0.));
#2368=DIRECTION('center_axis',(0.,0.,1.));
#2369=DIRECTION('ref_axis',(1.,0.,0.));
#2370=DIRECTION('center_axis',(0.,0.,1.));
#2371=DIRECTION('ref_axis',(1.,0.,0.));
#2372=DIRECTION('center_axis',(0.,0.,-1.));
#2373=DIRECTION('ref_axis',(1.,0.,0.));
#2374=DIRECTION('center_axis',(0.,0.,1.));
#2375=DIRECTION('ref_axis',(6.12323399573677E-17,-1.,0.));
#2376=DIRECTION('center_axis',(0.,0.,-1.));
#2377=DIRECTION('ref_axis',(1.,0.,0.));
#2378=DIRECTION('center_axis',(0.,0.,1.));
#2379=DIRECTION('ref_axis',(6.12323399573677E-17,-1.,0.));
#2380=DIRECTION('center_axis',(0.,0.,1.));
#2381=DIRECTION('ref_axis',(1.,0.,0.));
#2382=DIRECTION('center_axis',(0.,0.,1.));
#2383=DIRECTION('ref_axis',(1.,0.,0.));
#2384=DIRECTION('axis',(0.,0.,1.));
#2385=DIRECTION('refdir',(1.,0.,0.));
#2386=DIRECTION('center_axis',(0.,0.,1.));
#2387=DIRECTION('ref_axis',(1.,0.,0.));
#2388=DIRECTION('center_axis',(0.,0.,1.));
#2389=DIRECTION('ref_axis',(1.,0.,0.));
#2390=DIRECTION('',(0.,0.,-1.));
#2391=DIRECTION('center_axis',(0.,0.,1.));
#2392=DIRECTION('ref_axis',(1.,0.,0.));
#2393=DIRECTION('center_axis',(0.,0.,1.));
#2394=DIRECTION('ref_axis',(1.,0.,0.));
#2395=DIRECTION('center_axis',(0.,0.,1.));
#2396=DIRECTION('ref_axis',(1.,0.,0.));
#2397=DIRECTION('',(0.447213595499958,5.47678698264203E-17,-0.894427190999916));
#2398=DIRECTION('',(0.,0.,1.));
#2399=DIRECTION('',(1.,0.,0.));
#2400=DIRECTION('',(0.,0.,1.));
#2401=DIRECTION('',(1.,0.,0.));
#2402=DIRECTION('',(0.,0.,1.));
#2403=DIRECTION('',(1.,0.,0.));
#2404=DIRECTION('',(0.,0.,1.));
#2405=DIRECTION('',(2.22044604925031E-16,1.,0.));
#2406=DIRECTION('',(0.,0.,1.));
#2407=DIRECTION('',(2.22044604925031E-16,1.,0.));
#2408=DIRECTION('',(0.,0.,1.));
#2409=DIRECTION('',(1.,0.,0.));
#2410=DIRECTION('',(0.,0.,1.));
#2411=DIRECTION('',(1.,0.,0.));
#2412=DIRECTION('',(0.,0.,1.));
#2413=DIRECTION('',(1.,0.,0.));
#2414=DIRECTION('',(0.,0.,1.));
#2415=DIRECTION('',(1.,0.,0.));
#2416=DIRECTION('',(0.,0.,1.));
#2417=DIRECTION('',(1.,0.,0.));
#2418=DIRECTION('',(0.,0.,1.));
#2419=DIRECTION('',(1.,0.,0.));
#2420=DIRECTION('',(0.,0.,1.));
#2421=DIRECTION('',(1.,0.,0.));
#2422=DIRECTION('',(0.,0.,1.));
#2423=DIRECTION('',(1.,0.,0.));
#2424=DIRECTION('',(0.,0.,1.));
#2425=DIRECTION('',(1.,0.,0.));
#2426=DIRECTION('',(0.,0.,1.));
#2427=DIRECTION('',(1.,0.,0.));
#2428=DIRECTION('',(0.,0.,1.));
#2429=DIRECTION('',(1.,0.,0.));
#2430=DIRECTION('',(0.,0.,1.));
#2431=DIRECTION('',(1.,0.,0.));
#2432=DIRECTION('',(0.,0.,1.));
#2433=DIRECTION('',(1.,0.,0.));
#2434=DIRECTION('',(0.,0.,1.));
#2435=DIRECTION('',(1.,0.,0.));
#2436=DIRECTION('',(0.,0.,1.));
#2437=DIRECTION('',(1.,0.,0.));
#2438=DIRECTION('',(0.,0.,1.));
#2439=DIRECTION('',(1.,0.,0.));
#2440=DIRECTION('',(0.,0.,1.));
#2441=DIRECTION('',(1.,0.,0.));
#2442=DIRECTION('',(0.,0.,1.));
#2443=DIRECTION('',(1.,0.,0.));
#2444=DIRECTION('',(0.,0.,1.));
#2445=DIRECTION('',(1.,0.,0.));
#2446=DIRECTION('',(0.,0.,1.));
#2447=DIRECTION('',(1.,0.,0.));
#2448=DIRECTION('',(0.,0.,1.));
#2449=DIRECTION('',(1.,0.,0.));
#2450=DIRECTION('',(0.,0.,1.));
#2451=DIRECTION('',(1.,0.,0.));
#2452=DIRECTION('',(0.,0.,1.));
#2453=DIRECTION('',(1.,0.,0.));
#2454=DIRECTION('',(0.,0.,1.));
#2455=DIRECTION('',(1.,0.,0.));
#2456=DIRECTION('',(0.,0.,1.));
#2457=DIRECTION('',(1.,0.,0.));
#2458=DIRECTION('',(0.,0.,1.));
#2459=DIRECTION('',(1.,0.,0.));
#2460=DIRECTION('',(0.,0.,1.));
#2461=DIRECTION('',(1.,0.,0.));
#2462=DIRECTION('',(0.,0.,1.));
#2463=DIRECTION('',(1.,0.,0.));
#2464=DIRECTION('',(0.,0.,1.));
#2465=DIRECTION('',(1.,0.,0.));
#2466=DIRECTION('',(0.,0.,1.));
#2467=DIRECTION('',(1.,0.,0.));
#2468=DIRECTION('',(0.,0.,1.));
#2469=DIRECTION('',(1.,0.,0.));
#2470=DIRECTION('',(0.,0.,1.));
#2471=DIRECTION('',(1.,0.,0.));
#2472=CARTESIAN_POINT('',(0.,0.,0.));
#2473=CARTESIAN_POINT('',(0.,0.,0.));
#2474=CARTESIAN_POINT('Origin',(25.,-15.,5.));
#2475=CARTESIAN_POINT('',(20.5,-15.,10.));
#2476=CARTESIAN_POINT('Origin',(25.,-15.,10.));
#2477=CARTESIAN_POINT('',(20.5,-15.,0.));
#2478=CARTESIAN_POINT('',(20.5,-15.,5.));
#2479=CARTESIAN_POINT('Origin',(25.,-15.,0.));
#2480=CARTESIAN_POINT('Origin',(-25.,-15.,5.));
#2481=CARTESIAN_POINT('',(-29.5,-15.,10.));
#2482=CARTESIAN_POINT('Origin',(-25.,-15.,10.));
#2483=CARTESIAN_POINT('',(-29.5,-15.,0.));
#2484=CARTESIAN_POINT('',(-29.5,-15.,5.));
#2485=CARTESIAN_POINT('Origin',(-25.,-15.,0.));
#2486=CARTESIAN_POINT('Origin',(-25.,15.,5.));
#2487=CARTESIAN_POINT('',(-29.5,15.,10.));
#2488=CARTESIAN_POINT('Origin',(-25.,15.,10.));
#2489=CARTESIAN_POINT('',(-29.5,15.,0.));
#2490=CARTESIAN_POINT('',(-29.5,15.,5.));
#2491=CARTESIAN_POINT('Origin',(-25.,15.,0.));
#2492=CARTESIAN_POINT('Origin',(25.,15.,5.));
#2493=CARTESIAN_POINT('',(20.5,15.,10.));
#2494=CARTESIAN_POINT('Origin',(25.,15.,10.));
#2495=CARTESIAN_POINT('',(20.5,15.,0.));
#2496=CARTESIAN_POINT('',(20.5,15.,5.));
#2497=CARTESIAN_POINT('Origin',(25.,15.,0.));
#2498=CARTESIAN_POINT('Origin',(0.,0.,5.));
#2499=CARTESIAN_POINT('',(-5.,6.12323399573677E-16,10.));
#2500=CARTESIAN_POINT('Origin',(0.,0.,10.));
#2501=CARTESIAN_POINT('',(-5.,6.12323399573677E-16,0.));
#2502=CARTESIAN_POINT('',(-5.,6.12323399573677E-16,5.));
#2503=CARTESIAN_POINT('Origin',(0.,0.,0.));
#2504=CARTESIAN_POINT('Origin',(40.,30.,0.));
#2505=CARTESIAN_POINT('',(40.,30.,0.));
#2506=CARTESIAN_POINT('',(-40.,30.,0.));
#2507=CARTESIAN_POINT('',(40.,30.,0.));
#2508=CARTESIAN_POINT('',(-40.,30.,10.));
#2509=CARTESIAN_POINT('',(-40.,30.,0.));
#2510=CARTESIAN_POINT('',(40.,30.,10.));
#2511=CARTESIAN_POINT('',(40.,30.,10.));
#2512=CARTESIAN_POINT('',(40.,30.,0.));
#2513=CARTESIAN_POINT('Origin',(40.,-30.,0.));
#2514=CARTESIAN_POINT('',(40.,-30.,0.));
#2515=CARTESIAN_POINT('',(40.,-30.,0.));
#2516=CARTESIAN_POINT('',(40.,-30.,10.));
#2517=CARTESIAN_POINT('',(40.,-30.,10.));
#2518=CARTESIAN_POINT('',(40.,-30.,0.));
#2519=CARTESIAN_POINT('Origin',(-40.,-30.,0.));
#2520=CARTESIAN_POINT('',(-40.,-30.,0.));
#2521=CARTESIAN_POINT('',(-40.,-30.,0.));
#2522=CARTESIAN_POINT('',(-40.,-30.,10.));
#2523=CARTESIAN_POINT('',(-40.,-30.,10.));
#2524=CARTESIAN_POINT('',(-40.,-30.,0.));
#2525=CARTESIAN_POINT('Origin',(-40.,30.,0.));
#2526=CARTESIAN_POINT('',(-40.,30.,0.));
#2527=CARTESIAN_POINT('',(-40.,30.,10.));
#2528=CARTESIAN_POINT('Origin',(0.,0.,10.));
#2529=CARTESIAN_POINT('Origin',(0.,0.,0.));
#2530=CARTESIAN_POINT('',(0.,0.,0.));
#2531=CARTESIAN_POINT('Origin',(0.,0.,0.));
#2532=CARTESIAN_POINT('',(-5.,-6.12323399573677E-16,10.));
#2533=CARTESIAN_POINT('Origin',(0.,0.,10.));
#2534=CARTESIAN_POINT('',(-5.,-6.12323399573677E-16,0.));
#2535=CARTESIAN_POINT('',(-5.,-6.12323399573677E-16,0.));
#2536=CARTESIAN_POINT('Origin',(0.,0.,0.));
#2537=CARTESIAN_POINT('Origin',(0.,0.,0.));
#2538=CARTESIAN_POINT('',(-12.,-1.46957615897682E-15,10.));
#2539=CARTESIAN_POINT('Origin',(0.,0.,10.));
#2540=CARTESIAN_POINT('',(-12.,-1.46957615897682E-15,0.));
#2541=CARTESIAN_POINT('',(-12.,-1.46957615897682E-15,0.));
#2542=CARTESIAN_POINT('Origin',(0.,0.,0.));
#2543=CARTESIAN_POINT('Origin',(0.,0.,10.));
#2544=CARTESIAN_POINT('Origin',(0.,0.,0.));
#2545=CARTESIAN_POINT('',(0.,0.,0.));
#2546=CARTESIAN_POINT('Origin',(120.,0.,4.));
#2547=CARTESIAN_POINT('',(113.,8.57252759403147E-16,8.));
#2548=CARTESIAN_POINT('Origin',(120.,0.,8.));
#2549=CARTESIAN_POINT('',(113.,8.57252759403147E-16,0.));
#2550=CARTESIAN_POINT('',(113.,8.57252759403147E-16,4.));
#2551=CARTESIAN_POINT('Origin',(120.,0.,0.));
#2552=CARTESIAN_POINT('Origin',(0.,0.,4.));
#2553=CARTESIAN_POINT('',(-7.,8.57252759403147E-16,8.));
#2554=CARTESIAN_POINT('Origin',(0.,0.,8.));
#2555=CARTESIAN_POINT('',(-7.,8.57252759403147E-16,0.));
#2556=CARTESIAN_POINT('',(-7.,8.57252759403147E-16,4.));
#2557=CARTESIAN_POINT('Origin',(0.,0.,0.));
#2558=CARTESIAN_POINT('Origin',(240.,0.,4.));
#2559=CARTESIAN_POINT('',(233.,8.57252759403147E-16,8.));
#2560=CARTESIAN_POINT('Origin',(240.,0.,8.));
#2561=CARTESIAN_POINT('',(233.,8.57252759403147E-16,0.));
#2562=CARTESIAN_POINT('',(233.,8.57252759403147E-16,4.));
#2563=CARTESIAN_POINT('Origin',(240.,0.,0.));
#2564=CARTESIAN_POINT('Origin',(240.,12.,0.));
#2565=CARTESIAN_POINT('',(240.,12.,0.));
#2566=CARTESIAN_POINT('',(0.,12.,0.));
#2567=CARTESIAN_POINT('',(240.,12.,0.));
#2568=CARTESIAN_POINT('',(0.,12.,8.));
#2569=CARTESIAN_POINT('',(0.,12.,0.));
#2570=CARTESIAN_POINT('',(240.,12.,8.));
#2571=CARTESIAN_POINT('',(240.,12.,8.));
#2572=CARTESIAN_POINT('',(240.,12.,0.));
#2573=CARTESIAN_POINT('Origin',(240.,-1.11022302462516E-15,0.));
#2574=CARTESIAN_POINT('',(240.,-12.,0.));
#2575=CARTESIAN_POINT('Origin',(240.,-1.11022302462516E-15,0.));
#2576=CARTESIAN_POINT('',(240.,-12.,8.));
#2577=CARTESIAN_POINT('Origin',(240.,-1.11022302462516E-15,8.));
#2578=CARTESIAN_POINT('',(240.,-12.,0.));
#2579=CARTESIAN_POINT('Origin',(0.,-12.,0.));
#2580=CARTESIAN_POINT('',(-1.46957615897682E-15,-12.,0.));
#2581=CARTESIAN_POINT('',(0.,-12.,0.));
#2582=CARTESIAN_POINT('',(-1.46957615897682E-15,-12.,8.));
#2583=CARTESIAN_POINT('',(0.,-12.,8.));
#2584=CARTESIAN_POINT('',(-1.46957615897682E-15,-12.,0.));
#2585=CARTESIAN_POINT('Origin',(0.,0.,0.));
#2586=CARTESIAN_POINT('Origin',(0.,0.,0.));
#2587=CARTESIAN_POINT('Origin',(0.,0.,8.));
#2588=CARTESIAN_POINT('Origin',(120.,0.,8.));
#2589=CARTESIAN_POINT('Origin',(120.,0.,0.));
#2590=CARTESIAN_POINT('',(0.,0.,0.));
#2591=CARTESIAN_POINT('Origin',(60.,0.,4.));
#2592=CARTESIAN_POINT('',(54.,7.34788079488412E-16,8.));
#2593=CARTESIAN_POINT('Origin',(60.,0.,8.));
#2594=CARTESIAN_POINT('',(54.,7.34788079488412E-16,0.));
#2595=CARTESIAN_POINT('',(54.,7.34788079488412E-16,4.));
#2596=CARTESIAN_POINT('Origin',(60.,0.,0.));
#2597=CARTESIAN_POINT('Origin',(0.,0.,4.));
#2598=CARTESIAN_POINT('',(-7.,8.57252759403147E-16,8.));
#2599=CARTESIAN_POINT('Origin',(0.,0.,8.));
#2600=CARTESIAN_POINT('',(-7.,8.57252759403147E-16,0.));
#2601=CARTESIAN_POINT('',(-7.,8.57252759403147E-16,4.));
#2602=CARTESIAN_POINT('Origin',(0.,0.,0.));
#2603=CARTESIAN_POINT('Origin',(120.,0.,4.));
#2604=CARTESIAN_POINT('',(113.,8.57252759403147E-16,8.));
#2605=CARTESIAN_POINT('Origin',(120.,0.,8.));
#2606=CARTESIAN_POINT('',(113.,8.57252759403147E-16,0.));
#2607=CARTESIAN_POINT('',(113.,8.57252759403147E-16,4.));
#2608=CARTESIAN_POINT('Origin',(120.,0.,0.));
#2609=CARTESIAN_POINT('Origin',(120.,12.,0.));
#2610=CARTESIAN_POINT('',(120.,12.,0.));
#2611=CARTESIAN_POINT('',(0.,12.,0.));
#2612=CARTESIAN_POINT('',(120.,12.,0.));
#2613=CARTESIAN_POINT('',(0.,12.,8.));
#2614=CARTESIAN_POINT('',(0.,12.,0.));
#2615=CARTESIAN_POINT('',(120.,12.,8.));
#2616=CARTESIAN_POINT('',(120.,12.,8.));
#2617=CARTESIAN_POINT('',(120.,12.,0.));
#2618=CARTESIAN_POINT('Origin',(120.,-1.11022302462516E-15,0.));
#2619=CARTESIAN_POINT('',(120.,-12.,0.));
#2620=CARTESIAN_POINT('Origin',(120.,-1.11022302462516E-15,0.));
#2621=CARTESIAN_POINT('',(120.,-12.,8.));
#2622=CARTESIAN_POINT('Origin',(120.,-1.11022302462516E-15,8.));
#2623=CARTESIAN_POINT('',(120.,-12.,0.));
#2624=CARTESIAN_POINT('Origin',(0.,-12.,0.));
#2625=CARTESIAN_POINT('',(-1.46957615897682E-15,-12.,0.));
#2626=CARTESIAN_POINT('',(0.,-12.,0.));
#2627=CARTESIAN_POINT('',(-1.46957615897682E-15,-12.,8.));
#2628=CARTESIAN_POINT('',(0.,-12.,8.));
#2629=CARTESIAN_POINT('',(-1.46957615897682E-15,-12.,0.));
#2630=CARTESIAN_POINT('Origin',(0.,0.,0.));
#2631=CARTESIAN_POINT('Origin',(0.,0.,0.));
#2632=CARTESIAN_POINT('Origin',(0.,0.,8.));
#2633=CARTESIAN_POINT('Origin',(60.,0.,8.));
#2634=CARTESIAN_POINT('Origin',(60.,0.,0.));
#2635=CARTESIAN_POINT('',(0.,0.,0.));
#2636=CARTESIAN_POINT('Origin',(0.,0.,31.));
#2637=CARTESIAN_POINT('',(-4.,-4.89858719658941E-16,30.));
#2638=CARTESIAN_POINT('Origin',(0.,0.,30.));
#2639=CARTESIAN_POINT('',(-4.,-4.89858719658941E-16,32.));
#2640=CARTESIAN_POINT('',(-4.,-4.89858719658941E-16,31.));
#2641=CARTESIAN_POINT('Origin',(0.,0.,32.));
#2642=CARTESIAN_POINT('Origin',(8.,0.,30.));
#2643=CARTESIAN_POINT('',(-5.,6.12323399573677E-16,30.));
#2644=CARTESIAN_POINT('Origin',(0.,0.,30.));
#2645=CARTESIAN_POINT('Origin',(4.,0.,32.));
#2646=CARTESIAN_POINT('',(-5.,-6.12323399573677E-16,32.));
#2647=CARTESIAN_POINT('Origin',(0.,0.,32.));
#2648=CARTESIAN_POINT('Origin',(0.,0.,0.));
#2649=CARTESIAN_POINT('',(-5.,-6.12323399573677E-16,33.));
#2650=CARTESIAN_POINT('Origin',(0.,0.,33.));
#2651=CARTESIAN_POINT('',(-5.,-6.12323399573677E-16,0.));
#2652=CARTESIAN_POINT('Origin',(0.,0.,0.));
#2653=CARTESIAN_POINT('',(-8.,-9.79717439317883E-16,0.));
#2654=CARTESIAN_POINT('Origin',(0.,0.,0.));
#2655=CARTESIAN_POINT('',(-5.,-6.12323399573677E-16,0.));
#2656=CARTESIAN_POINT('Origin',(0.,0.,0.));
#2657=CARTESIAN_POINT('Origin',(0.,0.,-4.));
#2658=CARTESIAN_POINT('',(-8.,-9.79717439317883E-16,-4.));
#2659=CARTESIAN_POINT('',(-8.,-9.79717439317883E-16,-4.));
#2660=CARTESIAN_POINT('Origin',(0.,0.,-4.));
#2661=CARTESIAN_POINT('Origin',(0.,0.,-4.));
#2662=CARTESIAN_POINT('Origin',(0.,0.,0.));
#2663=CARTESIAN_POINT('',(-5.,-6.12323399573677E-16,0.));
#2664=CARTESIAN_POINT('Origin',(0.,0.,33.));
#2665=CARTESIAN_POINT('',(0.,0.,0.));
#2666=CARTESIAN_POINT('Origin',(0.,0.,21.));
#2667=CARTESIAN_POINT('',(-4.,-4.89858719658941E-16,20.));
#2668=CARTESIAN_POINT('Origin',(0.,0.,20.));
#2669=CARTESIAN_POINT('',(-4.,-4.89858719658941E-16,22.));
#2670=CARTESIAN_POINT('',(-4.,-4.89858719658941E-16,21.));
#2671=CARTESIAN_POINT('Origin',(0.,0.,22.));
#2672=CARTESIAN_POINT('Origin',(8.,0.,20.));
#2673=CARTESIAN_POINT('',(-5.,6.12323399573677E-16,20.));
#2674=CARTESIAN_POINT('Origin',(0.,0.,20.));
#2675=CARTESIAN_POINT('Origin',(4.,0.,22.));
#2676=CARTESIAN_POINT('',(-5.,-6.12323399573677E-16,22.));
#2677=CARTESIAN_POINT('Origin',(0.,0.,22.));
#2678=CARTESIAN_POINT('Origin',(0.,0.,0.));
#2679=CARTESIAN_POINT('',(-5.,-6.12323399573677E-16,23.));
#2680=CARTESIAN_POINT('Origin',(0.,0.,23.));
#2681=CARTESIAN_POINT('',(-5.,-6.12323399573677E-16,0.));
#2682=CARTESIAN_POINT('Origin',(0.,0.,0.));
#2683=CARTESIAN_POINT('',(-8.,-9.79717439317883E-16,0.));
#2684=CARTESIAN_POINT('Origin',(0.,0.,0.));
#2685=CARTESIAN_POINT('',(-5.,-6.12323399573677E-16,0.));
#2686=CARTESIAN_POINT('Origin',(0.,0.,0.));
#2687=CARTESIAN_POINT('Origin',(0.,0.,-2.));
#2688=CARTESIAN_POINT('',(-8.,-9.79717439317883E-16,-2.));
#2689=CARTESIAN_POINT('',(-8.,-9.79717439317883E-16,-2.));
#2690=CARTESIAN_POINT('Origin',(0.,0.,-2.));
#2691=CARTESIAN_POINT('Origin',(0.,0.,-2.));
#2692=CARTESIAN_POINT('',(-2.,-2.44929359829471E-16,-2.));
#2693=CARTESIAN_POINT('Origin',(0.,0.,-2.));
#2694=CARTESIAN_POINT('Origin',(0.,0.,0.));
#2695=CARTESIAN_POINT('',(-2.,-2.44929359829471E-16,23.));
#2696=CARTESIAN_POINT('Origin',(0.,0.,23.));
#2697=CARTESIAN_POINT('',(-2.,-2.44929359829471E-16,0.));
#2698=CARTESIAN_POINT('Origin',(0.,0.,0.));
#2699=CARTESIAN_POINT('',(-5.,-6.12323399573677E-16,0.));
#2700=CARTESIAN_POINT('Origin',(0.,0.,23.));
#2701=CARTESIAN_POINT('',(0.,0.,0.));
#2702=CARTESIAN_POINT('Origin',(0.,0.,8.));
#2703=CARTESIAN_POINT('',(-8.,-9.79717439317883E-16,8.));
#2704=CARTESIAN_POINT('Origin',(0.,0.,8.));
#2705=CARTESIAN_POINT('',(-6.,-7.34788079488412E-16,8.));
#2706=CARTESIAN_POINT('Origin',(0.,0.,8.));
#2707=CARTESIAN_POINT('Origin',(0.,0.,8.));
#2708=CARTESIAN_POINT('',(-8.,-9.79717439317883E-16,12.));
#2709=CARTESIAN_POINT('Origin',(0.,0.,12.));
#2710=CARTESIAN_POINT('',(-8.,-9.79717439317883E-16,8.));
#2711=CARTESIAN_POINT('Origin',(0.,0.,12.));
#2712=CARTESIAN_POINT('',(-2.,-2.44929359829471E-16,12.));
#2713=CARTESIAN_POINT('Origin',(0.,0.,12.));
#2714=CARTESIAN_POINT('Origin',(0.,0.,0.));
#2715=CARTESIAN_POINT('',(-2.,-2.44929359829471E-16,0.));
#2716=CARTESIAN_POINT('',(-2.,-2.44929359829471E-16,0.));
#2717=CARTESIAN_POINT('Origin',(0.,0.,0.));
#2718=CARTESIAN_POINT('Origin',(0.,0.,0.));
#2719=CARTESIAN_POINT('',(-6.,-7.34788079488412E-16,0.));
#2720=CARTESIAN_POINT('',(-6.,-7.34788079488412E-16,0.));
#2721=CARTESIAN_POINT('Origin',(0.,0.,0.));
#2722=CARTESIAN_POINT('Origin',(0.,0.,0.));
#2723=CARTESIAN_POINT('',(0.,0.,0.));
#2724=CARTESIAN_POINT('Origin',(0.,0.,4.));
#2725=CARTESIAN_POINT('',(-7.,8.57252759403147E-16,8.));
#2726=CARTESIAN_POINT('Origin',(0.,0.,8.));
#2727=CARTESIAN_POINT('',(-7.,8.57252759403147E-16,0.));
#2728=CARTESIAN_POINT('',(-7.,8.57252759403147E-16,4.));
#2729=CARTESIAN_POINT('Origin',(0.,0.,0.));
#2730=CARTESIAN_POINT('Origin',(120.,0.,4.));
#2731=CARTESIAN_POINT('',(113.,8.57252759403147E-16,8.));
#2732=CARTESIAN_POINT('Origin',(120.,0.,8.));
#2733=CARTESIAN_POINT('',(113.,8.57252759403147E-16,0.));
#2734=CARTESIAN_POINT('',(113.,8.57252759403147E-16,4.));
#2735=CARTESIAN_POINT('Origin',(120.,0.,0.));
#2736=CARTESIAN_POINT('Origin',(120.,12.,0.));
#2737=CARTESIAN_POINT('',(120.,12.,0.));
#2738=CARTESIAN_POINT('',(0.,12.,0.));
#2739=CARTESIAN_POINT('',(120.,12.,0.));
#2740=CARTESIAN_POINT('',(0.,12.,8.));
#2741=CARTESIAN_POINT('',(0.,12.,0.));
#2742=CARTESIAN_POINT('',(120.,12.,8.));
#2743=CARTESIAN_POINT('',(120.,12.,8.));
#2744=CARTESIAN_POINT('',(120.,12.,0.));
#2745=CARTESIAN_POINT('Origin',(120.,-1.11022302462516E-15,0.));
#2746=CARTESIAN_POINT('',(120.,-12.,0.));
#2747=CARTESIAN_POINT('Origin',(120.,-1.11022302462516E-15,0.));
#2748=CARTESIAN_POINT('',(120.,-12.,8.));
#2749=CARTESIAN_POINT('Origin',(120.,-1.11022302462516E-15,8.));
#2750=CARTESIAN_POINT('',(120.,-12.,0.));
#2751=CARTESIAN_POINT('Origin',(0.,-12.,0.));
#2752=CARTESIAN_POINT('',(-1.46957615897682E-15,-12.,0.));
#2753=CARTESIAN_POINT('',(0.,-12.,0.));
#2754=CARTESIAN_POINT('',(-1.46957615897682E-15,-12.,8.));
#2755=CARTESIAN_POINT('',(0.,-12.,8.));
#2756=CARTESIAN_POINT('',(-1.46957615897682E-15,-12.,0.));
#2757=CARTESIAN_POINT('Origin',(0.,0.,0.));
#2758=CARTESIAN_POINT('Origin',(0.,0.,0.));
#2759=CARTESIAN_POINT('Origin',(0.,0.,8.));
#2760=CARTESIAN_POINT('Origin',(60.,0.,8.));
#2761=CARTESIAN_POINT('Origin',(60.,0.,0.));
#2762=CARTESIAN_POINT('',(0.,0.,0.));
#2763=CARTESIAN_POINT('Origin',(0.,0.,0.));
#2764=CARTESIAN_POINT('',(-5.,-6.12323399573677E-16,8.));
#2765=CARTESIAN_POINT('Origin',(0.,0.,8.));
#2766=CARTESIAN_POINT('',(-5.,-6.12323399573677E-16,0.));
#2767=CARTESIAN_POINT('',(-5.,-6.12323399573677E-16,0.));
#2768=CARTESIAN_POINT('Origin',(0.,0.,0.));
#2769=CARTESIAN_POINT('Origin',(0.,0.,0.));
#2770=CARTESIAN_POINT('',(-7.,-8.57252759403147E-16,8.));
#2771=CARTESIAN_POINT('Origin',(0.,0.,8.));
#2772=CARTESIAN_POINT('',(-7.,-8.57252759403147E-16,0.));
#2773=CARTESIAN_POINT('',(-7.,-8.57252759403147E-16,0.));
#2774=CARTESIAN_POINT('Origin',(0.,0.,0.));
#2775=CARTESIAN_POINT('Origin',(0.,0.,8.));
#2776=CARTESIAN_POINT('Origin',(0.,0.,0.));
#2777=CARTESIAN_POINT('',(0.,0.,0.));
#2778=CARTESIAN_POINT('Origin',(0.,0.,21.));
#2779=CARTESIAN_POINT('',(-4.,-4.89858719658941E-16,20.));
#2780=CARTESIAN_POINT('Origin',(0.,0.,20.));
#2781=CARTESIAN_POINT('',(-4.,-4.89858719658941E-16,22.));
#2782=CARTESIAN_POINT('',(-4.,-4.89858719658941E-16,21.));
#2783=CARTESIAN_POINT('Origin',(0.,0.,22.));
#2784=CARTESIAN_POINT('Origin',(8.,0.,20.));
#2785=CARTESIAN_POINT('',(-5.,6.12323399573677E-16,20.));
#2786=CARTESIAN_POINT('Origin',(0.,0.,20.));
#2787=CARTESIAN_POINT('Origin',(4.,0.,22.));
#2788=CARTESIAN_POINT('',(-5.,-6.12323399573677E-16,22.));
#2789=CARTESIAN_POINT('Origin',(0.,0.,22.));
#2790=CARTESIAN_POINT('Origin',(0.,0.,0.));
#2791=CARTESIAN_POINT('',(-5.,-6.12323399573677E-16,23.));
#2792=CARTESIAN_POINT('Origin',(0.,0.,23.));
#2793=CARTESIAN_POINT('',(-5.,-6.12323399573677E-16,0.));
#2794=CARTESIAN_POINT('Origin',(0.,0.,0.));
#2795=CARTESIAN_POINT('',(-8.,-9.79717439317883E-16,0.));
#2796=CARTESIAN_POINT('Origin',(0.,0.,0.));
#2797=CARTESIAN_POINT('',(-5.,-6.12323399573677E-16,0.));
#2798=CARTESIAN_POINT('Origin',(0.,0.,0.));
#2799=CARTESIAN_POINT('Origin',(0.,0.,-2.));
#2800=CARTESIAN_POINT('',(-8.,-9.79717439317883E-16,-2.));
#2801=CARTESIAN_POINT('',(-8.,-9.79717439317883E-16,-2.));
#2802=CARTESIAN_POINT('Origin',(0.,0.,-2.));
#2803=CARTESIAN_POINT('Origin',(0.,0.,-2.));
#2804=CARTESIAN_POINT('Origin',(0.,0.,0.));
#2805=CARTESIAN_POINT('',(-5.,-6.12323399573677E-16,0.));
#2806=CARTESIAN_POINT('Origin',(0.,0.,23.));
#2807=CARTESIAN_POINT('',(0.,0.,0.));
#2808=CARTESIAN_POINT('Origin',(0.,0.,0.));
#2809=CARTESIAN_POINT('',(-5.,-6.12323399573677E-16,2.));
#2810=CARTESIAN_POINT('Origin',(0.,0.,2.));
#2811=CARTESIAN_POINT('',(-5.,-6.12323399573677E-16,0.));
#2812=CARTESIAN_POINT('',(-5.,-6.12323399573677E-16,0.));
#2813=CARTESIAN_POINT('Origin',(0.,0.,0.));
#2814=CARTESIAN_POINT('Origin',(0.,0.,0.));
#2815=CARTESIAN_POINT('',(-10.,-1.22464679914735E-15,2.));
#2816=CARTESIAN_POINT('Origin',(0.,0.,2.));
#2817=CARTESIAN_POINT('',(-10.,-1.22464679914735E-15,0.));
#2818=CARTESIAN_POINT('',(-10.,-1.22464679914735E-15,0.));
#2819=CARTESIAN_POINT('Origin',(0.,0.,0.));
#2820=CARTESIAN_POINT('Origin',(0.,0.,2.));
#2821=CARTESIAN_POINT('Origin',(0.,0.,0.));
#2822=CARTESIAN_POINT('',(0.,0.,0.));
#2823=CARTESIAN_POINT('Origin',(-1.,0.,1.));
#2824=CARTESIAN_POINT('',(-1.,3.87298334620742,0.));
#2825=CARTESIAN_POINT('',(-1.,3.87298334620742,1.));
#2826=CARTESIAN_POINT('',(-1.,3.87298334620742,0.));
#2827=CARTESIAN_POINT('',(-1.,7.93725393319377,0.));
#2828=CARTESIAN_POINT('',(-1.,0.,0.));
#2829=CARTESIAN_POINT('',(-1.,7.93725393319377,1.));
#2830=CARTESIAN_POINT('',(-1.,7.93725393319377,0.));
#2831=CARTESIAN_POINT('',(-1.,0.,1.));
#2832=CARTESIAN_POINT('Origin',(1.,16.,1.));
#2833=CARTESIAN_POINT('',(1.,3.87298334620742,1.));
#2834=CARTESIAN_POINT('',(1.,3.87298334620742,0.));
#2835=CARTESIAN_POINT('',(1.,3.87298334620742,0.));
#2836=CARTESIAN_POINT('',(1.,7.93725393319377,1.));
#2837=CARTESIAN_POINT('',(1.,8.,1.));
#2838=CARTESIAN_POINT('',(1.,7.93725393319377,0.));
#2839=CARTESIAN_POINT('',(1.,7.93725393319377,0.));
#2840=CARTESIAN_POINT('',(1.,8.,0.));
#2841=CARTESIAN_POINT('Origin',(0.,0.,0.));
#2842=CARTESIAN_POINT('Origin',(0.,0.,0.));
#2843=CARTESIAN_POINT('Origin',(0.,0.,0.));
#2844=CARTESIAN_POINT('Origin',(0.,0.,0.));
#2845=CARTESIAN_POINT('Origin',(0.,0.,1.));
#2846=CARTESIAN_POINT('Origin',(0.,0.,0.));
#2847=CARTESIAN_POINT('Origin',(0.,0.,1.));
#2848=CARTESIAN_POINT('Origin',(0.,0.,1.));
#2849=CARTESIAN_POINT('',(0.,0.,0.));
#2850=CARTESIAN_POINT('Origin',(0.,0.,4.));
#2851=CARTESIAN_POINT('',(-2.,-2.44929359829471E-16,50.));
#2852=CARTESIAN_POINT('Origin',(0.,0.,50.));
#2853=CARTESIAN_POINT('',(-2.,-2.44929359829471E-16,4.));
#2854=CARTESIAN_POINT('',(-2.,-2.44929359829471E-16,4.));
#2855=CARTESIAN_POINT('Origin',(0.,0.,4.));
#2856=CARTESIAN_POINT('Origin',(0.,0.,50.));
#2857=CARTESIAN_POINT('Origin',(0.,0.,2.));
#2858=CARTESIAN_POINT('',(0.,0.,0.));
#2859=CARTESIAN_POINT('',(-1.,-1.22464679914735E-16,2.));
#2860=CARTESIAN_POINT('',(0.,0.,0.));
#2861=CARTESIAN_POINT('',(0.,0.,10.));
#2862=CARTESIAN_POINT('',(0.,0.,20.));
#2863=CARTESIAN_POINT('',(240.,0.,28.));
#2864=CARTESIAN_POINT('',(120.,0.,28.));
#2865=CARTESIAN_POINT('',(0.,0.,20.));
#2866=CARTESIAN_POINT('',(0.,0.,0.));
#2867=CARTESIAN_POINT('',(120.,0.,18.));
#2868=CARTESIAN_POINT('',(240.,120.,18.));
#2869=CARTESIAN_POINT('',(0.,0.,28.));
#2870=CARTESIAN_POINT('',(0.,0.,31.));
#2871=CARTESIAN_POINT('',(120.,60.,28.));
#2872=CARTESIAN_POINT('',(120.,60.,0.));
#2873=CARTESIAN_POINT('',(120.,120.,20.));
#2874=CARTESIAN_POINT('',(120.,0.,20.));
#2875=CARTESIAN_POINT('',(240.,0.,20.));
#2876=CARTESIAN_POINT('',(240.,0.,28.));
#2877=CARTESIAN_POINT('',(240.,120.,28.));
#2878=CARTESIAN_POINT('',(120.,120.,20.));
#2879=CARTESIAN_POINT('',(240.,120.,20.));
#2880=CARTESIAN_POINT('',(120.,0.,28.));
#2881=CARTESIAN_POINT('',(120.,120.,28.));
#2882=CARTESIAN_POINT('',(120.,0.,18.));
#2883=CARTESIAN_POINT('',(120.,0.,36.));
#2884=CARTESIAN_POINT('',(120.,0.,39.));
#2885=CARTESIAN_POINT('',(240.,0.,18.));
#2886=CARTESIAN_POINT('',(240.,0.,18.));
#2887=CARTESIAN_POINT('',(240.,0.,36.));
#2888=CARTESIAN_POINT('',(240.,0.,39.));
#2889=CARTESIAN_POINT('',(120.,120.,18.));
#2890=CARTESIAN_POINT('',(120.,120.,18.));
#2891=CARTESIAN_POINT('',(120.,120.,36.));
#2892=CARTESIAN_POINT('',(120.,120.,39.));
#2893=CARTESIAN_POINT('',(240.,120.,18.));
#2894=CARTESIAN_POINT('',(240.,120.,36.));
#2895=CARTESIAN_POINT('',(240.,120.,39.));
#2896=CARTESIAN_POINT('',(240.,120.,0.));
#2897=UNCERTAINTY_MEASURE_WITH_UNIT(LENGTH_MEASURE(0.01),#2927,
'DISTANCE_ACCURACY_VALUE',
'Maximum model space distance between geometric entities at asserted c
onnectivities');
#2898=UNCERTAINTY_MEASURE_WITH_UNIT(LENGTH_MEASURE(0.01),#2927,
'DISTANCE_ACCURACY_VALUE',
'Maximum model space distance between geometric entities at asserted c
onnectivities');
#2899=UNCERTAINTY_MEASURE_WITH_UNIT(LENGTH_MEASURE(0.01),#2927,
'DISTANCE_ACCURACY_VALUE',
'Maximum model space distance between geometric entities at asserted c
onnectivities');
#2900=UNCERTAINTY_MEASURE_WITH_UNIT(LENGTH_MEASURE(0.01),#2927,
'DISTANCE_ACCURACY_VALUE',
'Maximum model space distance between geometric entities at asserted c
onnectivities');
#2901=UNCERTAINTY_MEASURE_WITH_UNIT(LENGTH_MEASURE(0.01),#2927,
'DISTANCE_ACCURACY_VALUE',
'Maximum model space distance between geometric entities at asserted c
onnectivities');
#2902=UNCERTAINTY_MEASURE_WITH_UNIT(LENGTH_MEASURE(0.01),#2927,
'DISTANCE_ACCURACY_VALUE',
'Maximum model space distance between geometric entities at asserted c
onnectivities');
#2903=UNCERTAINTY_MEASURE_WITH_UNIT(LENGTH_MEASURE(0.01),#2927,
'DISTANCE_ACCURACY_VALUE',
'Maximum model space distance between geometric entities at asserted c
onnectivities');
#2904=UNCERTAINTY_MEASURE_WITH_UNIT(LENGTH_MEASURE(0.01),#2927,
'DISTANCE_ACCURACY_VALUE',
'Maximum model space distance between geometric entities at asserted c
onnectivities');
#2905=UNCERTAINTY_MEASURE_WITH_UNIT(LENGTH_MEASURE(0.01),#2927,
'DISTANCE_ACCURACY_VALUE',
'Maximum model space distance between geometric entities at asserted c
onnectivities');
#2906=UNCERTAINTY_MEASURE_WITH_UNIT(LENGTH_MEASURE(0.01),#2927,
'DISTANCE_ACCURACY_VALUE',
'Maximum model space distance between geometric entities at asserted c
onnectivities');
#2907=UNCERTAINTY_MEASURE_WITH_UNIT(LENGTH_MEASURE(0.01),#2927,
'DISTANCE_ACCURACY_VALUE',
'Maximum model space distance between geometric entities at asserted c
onnectivities');
#2908=UNCERTAINTY_MEASURE_WITH_UNIT(LENGTH_MEASURE(0.01),#2927,
'DISTANCE_ACCURACY_VALUE',
'Maximum model space distance between geometric entities at asserted c
onnectivities');
#2909=UNCERTAINTY_MEASURE_WITH_UNIT(LENGTH_MEASURE(0.01),#2927,
'DISTANCE_ACCURACY_VALUE',
'Maximum model space distance between geometric entities at asserted c
onnectivities');
#2910=UNCERTAINTY_MEASURE_WITH_UNIT(LENGTH_MEASURE(0.01),#2927,
'DISTANCE_ACCURACY_VALUE',
'Maximum model space distance between geometric entities at asserted c
onnectivities');
#2911=UNCERTAINTY_MEASURE_WITH_UNIT(LENGTH_MEASURE(0.01),#2927,
'DISTANCE_ACCURACY_VALUE',
'Maximum model space distance between geometric entities at asserted c
onnectivities');
#2912=(
GEOMETRIC_REPRESENTATION_CONTEXT(3)
GLOBAL_UNCERTAINTY_ASSIGNED_CONTEXT((#2897))
GLOBAL_UNIT_ASSIGNED_CONTEXT((#2927,#2929,#2930))
REPRESENTATION_CONTEXT('','3D')
);
#2913=(
GEOMETRIC_REPRESENTATION_CONTEXT(3)
GLOBAL_UNCERTAINTY_ASSIGNED_CONTEXT((#2898))
GLOBAL_UNIT_ASSIGNED_CONTEXT((#2927,#2929,#2930))
REPRESENTATION_CONTEXT('','3D')
);
#2914=(
GEOMETRIC_REPRESENTATION_CONTEXT(3)
GLOBAL_UNCERTAINTY_ASSIGNED_CONTEXT((#2899))
GLOBAL_UNIT_ASSIGNED_CONTEXT((#2927,#2929,#2930))
REPRESENTATION_CONTEXT('','3D')
);
#2915=(
GEOMETRIC_REPRESENTATION_CONTEXT(3)
GLOBAL_UNCERTAINTY_ASSIGNED_CONTEXT((#2900))
GLOBAL_UNIT_ASSIGNED_CONTEXT((#2927,#2929,#2930))
REPRESENTATION_CONTEXT('','3D')
);
#2916=(
GEOMETRIC_REPRESENTATION_CONTEXT(3)
GLOBAL_UNCERTAINTY_ASSIGNED_CONTEXT((#2901))
GLOBAL_UNIT_ASSIGNED_CONTEXT((#2927,#2929,#2930))
REPRESENTATION_CONTEXT('','3D')
);
#2917=(
GEOMETRIC_REPRESENTATION_CONTEXT(3)
GLOBAL_UNCERTAINTY_ASSIGNED_CONTEXT((#2902))
GLOBAL_UNIT_ASSIGNED_CONTEXT((#2927,#2929,#2930))
REPRESENTATION_CONTEXT('','3D')
);
#2918=(
GEOMETRIC_REPRESENTATION_CONTEXT(3)
GLOBAL_UNCERTAINTY_ASSIGNED_CONTEXT((#2903))
GLOBAL_UNIT_ASSIGNED_CONTEXT((#2927,#2929,#2930))
REPRESENTATION_CONTEXT('','3D')
);
#2919=(
GEOMETRIC_REPRESENTATION_CONTEXT(3)
GLOBAL_UNCERTAINTY_ASSIGNED_CONTEXT((#2904))
GLOBAL_UNIT_ASSIGNED_CONTEXT((#2927,#2929,#2930))
REPRESENTATION_CONTEXT('','3D')
);
#2920=(
GEOMETRIC_REPRESENTATION_CONTEXT(3)
GLOBAL_UNCERTAINTY_ASSIGNED_CONTEXT((#2905))
GLOBAL_UNIT_ASSIGNED_CONTEXT((#2927,#2929,#2930))
REPRESENTATION_CONTEXT('','3D')
);
#2921=(
GEOMETRIC_REPRESENTATION_CONTEXT(3)
GLOBAL_UNCERTAINTY_ASSIGNED_CONTEXT((#2906))
GLOBAL_UNIT_ASSIGNED_CONTEXT((#2927,#2929,#2930))
REPRESENTATION_CONTEXT('','3D')
);
#2922=(
GEOMETRIC_REPRESENTATION_CONTEXT(3)
GLOBAL_UNCERTAINTY_ASSIGNED_CONTEXT((#2907))
GLOBAL_UNIT_ASSIGNED_CONTEXT((#2927,#2929,#2930))
REPRESENTATION_CONTEXT('','3D')
);
#2923=(
GEOMETRIC_REPRESENTATION_CONTEXT(3)
GLOBAL_UNCERTAINTY_ASSIGNED_CONTEXT((#2908))
GLOBAL_UNIT_ASSIGNED_CONTEXT((#2927,#2929,#2930))
REPRESENTATION_CONTEXT('','3D')
);
#2924=(
GEOMETRIC_REPRESENTATION_CONTEXT(3)
GLOBAL_UNCERTAINTY_ASSIGNED_CONTEXT((#2909))
GLOBAL_UNIT_ASSIGNED_CONTEXT((#2927,#2929,#2930))
REPRESENTATION_CONTEXT('','3D')
);
#2925=(
GEOMETRIC_REPRESENTATION_CONTEXT(3)
GLOBAL_UNCERTAINTY_ASSIGNED_CONTEXT((#2910))
GLOBAL_UNIT_ASSIGNED_CONTEXT((#2927,#2929,#2930))
REPRESENTATION_CONTEXT('','3D')
);
#2926=(
GEOMETRIC_REPRESENTATION_CONTEXT(3)
GLOBAL_UNCERTAINTY_ASSIGNED_CONTEXT((#2911))
GLOBAL_UNIT_ASSIGNED_CONTEXT((#2927,#2929,#2930))
REPRESENTATION_CONTEXT('','3D')
);
#2927=(
LENGTH_UNIT()
NAMED_UNIT(*)
SI_UNIT(.MILLI.,.METRE.)
);
#2928=(
LENGTH_UNIT()
NAMED_UNIT(*)
SI_UNIT($,.METRE.)
);
#2929=(
NAMED_UNIT(*)
PLANE_ANGLE_UNIT()
SI_UNIT($,.RADIAN.)
);
#2930=(
NAMED_UNIT(*)
SI_UNIT($,.STERADIAN.)
SOLID_ANGLE_UNIT()
);
#2931=SHAPE_DEFINITION_REPRESENTATION(#2945,#2996);
#2932=SHAPE_DEFINITION_REPRESENTATION(#2946,#2997);
#2933=SHAPE_DEFINITION_REPRESENTATION(#2947,#2998);
#2934=SHAPE_DEFINITION_REPRESENTATION(#2948,#2999);
#2935=SHAPE_DEFINITION_REPRESENTATION(#2949,#3000);
#2936=SHAPE_DEFINITION_REPRESENTATION(#2950,#3001);
#2937=SHAPE_DEFINITION_REPRESENTATION(#2951,#3002);
#2938=SHAPE_DEFINITION_REPRESENTATION(#2952,#3003);
#2939=SHAPE_DEFINITION_REPRESENTATION(#2953,#3004);
#2940=SHAPE_DEFINITION_REPRESENTATION(#2954,#3005);
#2941=SHAPE_DEFINITION_REPRESENTATION(#2955,#3006);
#2942=SHAPE_DEFINITION_REPRESENTATION(#2956,#3007);
#2943=SHAPE_DEFINITION_REPRESENTATION(#2957,#3008);
#2944=SHAPE_DEFINITION_REPRESENTATION(#2958,#3009);
#2945=PRODUCT_DEFINITION_SHAPE('',$,#3011);
#2946=PRODUCT_DEFINITION_SHAPE('',$,#3012);
#2947=PRODUCT_DEFINITION_SHAPE('',$,#3013);
#2948=PRODUCT_DEFINITION_SHAPE('',$,#3014);
#2949=PRODUCT_DEFINITION_SHAPE('',$,#3015);
#2950=PRODUCT_DEFINITION_SHAPE('',$,#3016);
#2951=PRODUCT_DEFINITION_SHAPE('',$,#3017);
#2952=PRODUCT_DEFINITION_SHAPE('',$,#3018);
#2953=PRODUCT_DEFINITION_SHAPE('',$,#3019);
#2954=PRODUCT_DEFINITION_SHAPE('',$,#3020);
#2955=PRODUCT_DEFINITION_SHAPE('',$,#3021);
#2956=PRODUCT_DEFINITION_SHAPE('',$,#3022);
#2957=PRODUCT_DEFINITION_SHAPE('',$,#3023);
#2958=PRODUCT_DEFINITION_SHAPE('',$,#3024);
#2959=PRODUCT_DEFINITION_SHAPE($,$,#122);
#2960=PRODUCT_DEFINITION_SHAPE($,$,#123);
#2961=PRODUCT_DEFINITION_SHAPE($,$,#124);
#2962=PRODUCT_DEFINITION_SHAPE($,$,#125);
#2963=PRODUCT_DEFINITION_SHAPE($,$,#126);
#2964=PRODUCT_DEFINITION_SHAPE($,$,#127);
#2965=PRODUCT_DEFINITION_SHAPE($,$,#128);
#2966=PRODUCT_DEFINITION_SHAPE($,$,#129);
#2967=PRODUCT_DEFINITION_SHAPE($,$,#130);
#2968=PRODUCT_DEFINITION_SHAPE($,$,#131);
#2969=PRODUCT_DEFINITION_SHAPE($,$,#132);
#2970=PRODUCT_DEFINITION_SHAPE($,$,#133);
#2971=PRODUCT_DEFINITION_SHAPE($,$,#134);
#2972=PRODUCT_DEFINITION_SHAPE($,$,#135);
#2973=PRODUCT_DEFINITION_SHAPE($,$,#136);
#2974=PRODUCT_DEFINITION_SHAPE($,$,#137);
#2975=PRODUCT_DEFINITION_SHAPE($,$,#138);
#2976=PRODUCT_DEFINITION_SHAPE($,$,#139);
#2977=PRODUCT_DEFINITION_SHAPE($,$,#140);
#2978=PRODUCT_DEFINITION_SHAPE($,$,#141);
#2979=PRODUCT_DEFINITION_SHAPE($,$,#142);
#2980=PRODUCT_DEFINITION_SHAPE($,$,#143);
#2981=PRODUCT_DEFINITION_SHAPE($,$,#144);
#2982=PRODUCT_DEFINITION_SHAPE($,$,#145);
#2983=PRODUCT_DEFINITION_SHAPE($,$,#146);
#2984=PRODUCT_DEFINITION_SHAPE($,$,#147);
#2985=PRODUCT_DEFINITION_SHAPE($,$,#148);
#2986=PRODUCT_DEFINITION_SHAPE($,$,#149);
#2987=PRODUCT_DEFINITION_SHAPE($,$,#150);
#2988=PRODUCT_DEFINITION_SHAPE($,$,#151);
#2989=PRODUCT_DEFINITION_SHAPE($,$,#152);
#2990=PRODUCT_DEFINITION_SHAPE($,$,#153);
#2991=PRODUCT_DEFINITION_SHAPE($,$,#154);
#2992=PRODUCT_DEFINITION_SHAPE($,$,#155);
#2993=PRODUCT_DEFINITION_SHAPE($,$,#156);
#2994=PRODUCT_DEFINITION_SHAPE($,$,#157);
#2995=PRODUCT_DEFINITION_SHAPE($,$,#158);
#2996=SHAPE_REPRESENTATION('',(#1698,#1892,#1893,#1894,#1895,#1896,#1897,
#1898,#1899,#1900,#1901,#1902,#1903,#1904,#1905,#1906,#1907,#1908,#1909,
#1910,#1911,#1912,#1913,#1914,#1915,#1916,#1917,#1918,#1919,#1920,#1921,
#1922,#1923,#1924,#1925,#1926,#1927,#1928),#2912);
#2997=SHAPE_REPRESENTATION('',(#1699),#2913);
#2998=SHAPE_REPRESENTATION('',(#1721),#2914);
#2999=SHAPE_REPRESENTATION('',(#1730),#2915);
#3000=SHAPE_REPRESENTATION('',(#1750),#2916);
#3001=SHAPE_REPRESENTATION('',(#1770),#2917);
#3002=SHAPE_REPRESENTATION('',(#1788),#2918);
#3003=SHAPE_REPRESENTATION('',(#1809),#2919);
#3004=SHAPE_REPRESENTATION('',(#1822),#2920);
#3005=SHAPE_REPRESENTATION('',(#1839),#2921);
#3006=SHAPE_REPRESENTATION('',(#1848),#2922);
#3007=SHAPE_REPRESENTATION('',(#1866),#2923);
#3008=SHAPE_REPRESENTATION('',(#1875),#2924);
#3009=SHAPE_REPRESENTATION('',(#1886),#2925);
#3010=PRODUCT_DEFINITION_CONTEXT('part definition',#3054,'design');
#3011=PRODUCT_DEFINITION('BR-210','BR-210',#3025,#3010);
#3012=PRODUCT_DEFINITION('Base plate','Base plate',#3026,#3010);
#3013=PRODUCT_DEFINITION('Pivot pedestal','Pivot pedestal',#3027,#3010);
#3014=PRODUCT_DEFINITION('Extended link','Extended link',#3028,#3010);
#3015=PRODUCT_DEFINITION('Drawing link','Drawing link',#3029,#3010);
#3016=PRODUCT_DEFINITION('Ground pivot pin','Ground pivot pin',#3030,#3010);
#3017=PRODUCT_DEFINITION('Hollow pivot pin','Hollow pivot pin',#3031,#3010);
#3018=PRODUCT_DEFINITION('Stylus holder','Stylus holder',#3032,#3010);
#3019=PRODUCT_DEFINITION('Coupler link','Coupler link',#3033,#3010);
#3020=PRODUCT_DEFINITION('Pivot bushing','Pivot bushing',#3034,#3010);
#3021=PRODUCT_DEFINITION('Link pivot pin','Link pivot pin',#3035,#3010);
#3022=PRODUCT_DEFINITION('Pivot washer','Pivot washer',#3036,#3010);
#3023=PRODUCT_DEFINITION('Pivot retaining ring','Pivot retaining ring',
#3037,#3010);
#3024=PRODUCT_DEFINITION('Stylus','Stylus',#3038,#3010);
#3025=PRODUCT_DEFINITION_FORMATION('',$,#3056);
#3026=PRODUCT_DEFINITION_FORMATION('',$,#3057);
#3027=PRODUCT_DEFINITION_FORMATION('',$,#3058);
#3028=PRODUCT_DEFINITION_FORMATION('',$,#3059);
#3029=PRODUCT_DEFINITION_FORMATION('',$,#3060);
#3030=PRODUCT_DEFINITION_FORMATION('',$,#3061);
#3031=PRODUCT_DEFINITION_FORMATION('',$,#3062);
#3032=PRODUCT_DEFINITION_FORMATION('',$,#3063);
#3033=PRODUCT_DEFINITION_FORMATION('',$,#3064);
#3034=PRODUCT_DEFINITION_FORMATION('',$,#3065);
#3035=PRODUCT_DEFINITION_FORMATION('',$,#3066);
#3036=PRODUCT_DEFINITION_FORMATION('',$,#3067);
#3037=PRODUCT_DEFINITION_FORMATION('',$,#3068);
#3038=PRODUCT_DEFINITION_FORMATION('',$,#3069);
#3039=PRODUCT_RELATED_PRODUCT_CATEGORY('BR-210','BR-210',(#3056));
#3040=PRODUCT_RELATED_PRODUCT_CATEGORY('Base plate','Base plate',(#3057));
#3041=PRODUCT_RELATED_PRODUCT_CATEGORY('Pivot pedestal',
'Pivot pedestal',(#3058));
#3042=PRODUCT_RELATED_PRODUCT_CATEGORY('Extended link','Extended link',
(#3059));
#3043=PRODUCT_RELATED_PRODUCT_CATEGORY('Drawing link','Drawing link',(#3060));
#3044=PRODUCT_RELATED_PRODUCT_CATEGORY('Ground pivot pin',
'Ground pivot pin',(#3061));
#3045=PRODUCT_RELATED_PRODUCT_CATEGORY('Hollow pivot pin',
'Hollow pivot pin',(#3062));
#3046=PRODUCT_RELATED_PRODUCT_CATEGORY('Stylus holder','Stylus holder',
(#3063));
#3047=PRODUCT_RELATED_PRODUCT_CATEGORY('Coupler link','Coupler link',(#3064));
#3048=PRODUCT_RELATED_PRODUCT_CATEGORY('Pivot bushing','Pivot bushing',
(#3065));
#3049=PRODUCT_RELATED_PRODUCT_CATEGORY('Link pivot pin',
'Link pivot pin',(#3066));
#3050=PRODUCT_RELATED_PRODUCT_CATEGORY('Pivot washer','Pivot washer',(#3067));
#3051=PRODUCT_RELATED_PRODUCT_CATEGORY('Pivot retaining ring',
'Pivot retaining ring',(#3068));
#3052=PRODUCT_RELATED_PRODUCT_CATEGORY('Stylus','Stylus',(#3069));
#3053=APPLICATION_PROTOCOL_DEFINITION('international standard',
'automotive_design',2009,#3054);
#3054=APPLICATION_CONTEXT(
'Core Data for Automotive Mechanical Design Process');
#3055=PRODUCT_CONTEXT('part definition',#3054,'mechanical');
#3056=PRODUCT('BR-210','BR-210',
'Independent 1:2 reduction pantograph. 120 mm parallelogram sides; fix
ed fulcrum on the extension of a 240 mm link. Drawing point halfway al
ong its link, so its XY displacement is one half of the tracing point.
 Replaceable pivot bushes and retained pins. Calibration and productio
n accuracy unassigned.',(#3055));
#3057=PRODUCT('Base plate','Base plate','Base plate',(#3055));
#3058=PRODUCT('Pivot pedestal','Pivot pedestal','Pivot pedestal',(#3055));
#3059=PRODUCT('Extended link','Extended link',$,(#3055));
#3060=PRODUCT('Drawing link','Drawing link',$,(#3055));
#3061=PRODUCT('Ground pivot pin','Ground pivot pin',$,(#3055));
#3062=PRODUCT('Hollow pivot pin','Hollow pivot pin',$,(#3055));
#3063=PRODUCT('Stylus holder','Stylus holder',$,(#3055));
#3064=PRODUCT('Coupler link','Coupler link',$,(#3055));
#3065=PRODUCT('Pivot bushing','Pivot bushing',$,(#3055));
#3066=PRODUCT('Link pivot pin','Link pivot pin',$,(#3055));
#3067=PRODUCT('Pivot washer','Pivot washer',$,(#3055));
#3068=PRODUCT('Pivot retaining ring','Pivot retaining ring',$,(#3055));
#3069=PRODUCT('Stylus','Stylus',$,(#3055));
#3070=PRESENTATION_STYLE_ASSIGNMENT((#3082));
#3071=PRESENTATION_STYLE_ASSIGNMENT((#3083));
#3072=PRESENTATION_STYLE_ASSIGNMENT((#3084));
#3073=PRESENTATION_STYLE_ASSIGNMENT((#3085));
#3074=PRESENTATION_STYLE_ASSIGNMENT((#3086));
#3075=PRESENTATION_STYLE_ASSIGNMENT((#3087));
#3076=PRESENTATION_STYLE_ASSIGNMENT((#3088));
#3077=PRESENTATION_STYLE_ASSIGNMENT((#3089));
#3078=PRESENTATION_STYLE_ASSIGNMENT((#3090));
#3079=PRESENTATION_STYLE_ASSIGNMENT((#3091));
#3080=PRESENTATION_STYLE_ASSIGNMENT((#3092));
#3081=PRESENTATION_STYLE_ASSIGNMENT((#3093));
#3082=SURFACE_STYLE_USAGE(.BOTH.,#3094);
#3083=SURFACE_STYLE_USAGE(.BOTH.,#3095);
#3084=SURFACE_STYLE_USAGE(.BOTH.,#3096);
#3085=SURFACE_STYLE_USAGE(.BOTH.,#3097);
#3086=SURFACE_STYLE_USAGE(.BOTH.,#3098);
#3087=SURFACE_STYLE_USAGE(.BOTH.,#3099);
#3088=SURFACE_STYLE_USAGE(.BOTH.,#3100);
#3089=SURFACE_STYLE_USAGE(.BOTH.,#3101);
#3090=SURFACE_STYLE_USAGE(.BOTH.,#3102);
#3091=SURFACE_STYLE_USAGE(.BOTH.,#3103);
#3092=SURFACE_STYLE_USAGE(.BOTH.,#3104);
#3093=SURFACE_STYLE_USAGE(.BOTH.,#3105);
#3094=SURFACE_SIDE_STYLE('',(#3106));
#3095=SURFACE_SIDE_STYLE('',(#3107));
#3096=SURFACE_SIDE_STYLE('',(#3108));
#3097=SURFACE_SIDE_STYLE('',(#3109));
#3098=SURFACE_SIDE_STYLE('',(#3110));
#3099=SURFACE_SIDE_STYLE('',(#3111));
#3100=SURFACE_SIDE_STYLE('',(#3112));
#3101=SURFACE_SIDE_STYLE('',(#3113));
#3102=SURFACE_SIDE_STYLE('',(#3114));
#3103=SURFACE_SIDE_STYLE('',(#3115));
#3104=SURFACE_SIDE_STYLE('',(#3116));
#3105=SURFACE_SIDE_STYLE('',(#3117));
#3106=SURFACE_STYLE_FILL_AREA(#3118);
#3107=SURFACE_STYLE_FILL_AREA(#3119);
#3108=SURFACE_STYLE_FILL_AREA(#3120);
#3109=SURFACE_STYLE_FILL_AREA(#3121);
#3110=SURFACE_STYLE_FILL_AREA(#3122);
#3111=SURFACE_STYLE_FILL_AREA(#3123);
#3112=SURFACE_STYLE_FILL_AREA(#3124);
#3113=SURFACE_STYLE_FILL_AREA(#3125);
#3114=SURFACE_STYLE_FILL_AREA(#3126);
#3115=SURFACE_STYLE_FILL_AREA(#3127);
#3116=SURFACE_STYLE_FILL_AREA(#3128);
#3117=SURFACE_STYLE_FILL_AREA(#3129);
#3118=FILL_AREA_STYLE('Steel - Satin',(#3130));
#3119=FILL_AREA_STYLE('Base gray',(#3131));
#3120=FILL_AREA_STYLE('Pedestal gray',(#3132));
#3121=FILL_AREA_STYLE('Extended link finish',(#3133));
#3122=FILL_AREA_STYLE('Drawing link finish',(#3134));
#3123=FILL_AREA_STYLE('Pivot gray',(#3135));
#3124=FILL_AREA_STYLE('Holder gray',(#3136));
#3125=FILL_AREA_STYLE('Coupler link finish',(#3137));
#3126=FILL_AREA_STYLE('Bearing light gray',(#3138));
#3127=FILL_AREA_STYLE('Washer light gray',(#3139));
#3128=FILL_AREA_STYLE('Dark gray',(#3140));
#3129=FILL_AREA_STYLE('Stylus light gray',(#3141));
#3130=FILL_AREA_STYLE_COLOUR('Steel - Satin',#3142);
#3131=FILL_AREA_STYLE_COLOUR('Base gray',#3143);
#3132=FILL_AREA_STYLE_COLOUR('Pedestal gray',#3144);
#3133=FILL_AREA_STYLE_COLOUR('Extended link finish',#3145);
#3134=FILL_AREA_STYLE_COLOUR('Drawing link finish',#3146);
#3135=FILL_AREA_STYLE_COLOUR('Pivot gray',#3147);
#3136=FILL_AREA_STYLE_COLOUR('Holder gray',#3148);
#3137=FILL_AREA_STYLE_COLOUR('Coupler link finish',#3149);
#3138=FILL_AREA_STYLE_COLOUR('Bearing light gray',#3150);
#3139=FILL_AREA_STYLE_COLOUR('Washer light gray',#3151);
#3140=FILL_AREA_STYLE_COLOUR('Dark gray',#3152);
#3141=FILL_AREA_STYLE_COLOUR('Stylus light gray',#3153);
#3142=COLOUR_RGB('Steel - Satin',0.627450980392157,0.627450980392157,0.627450980392157);
#3143=COLOUR_RGB('Base gray',0.407843137254902,0.447058823529412,0.498039215686275);
#3144=COLOUR_RGB('Pedestal gray',0.407843137254902,0.447058823529412,0.498039215686275);
#3145=COLOUR_RGB('Extended link finish',0.0901960784313725,0.270588235294118,
0.513725490196078);
#3146=COLOUR_RGB('Drawing link finish',0.662745098039216,0.831372549019608,
0.949019607843137);
#3147=COLOUR_RGB('Pivot gray',0.407843137254902,0.447058823529412,0.498039215686275);
#3148=COLOUR_RGB('Holder gray',0.407843137254902,0.447058823529412,0.498039215686275);
#3149=COLOUR_RGB('Coupler link finish',0.317647058823529,0.686274509803922,
0.890196078431372);
#3150=COLOUR_RGB('Bearing light gray',0.725490196078431,0.752941176470588,
0.792156862745098);
#3151=COLOUR_RGB('Washer light gray',0.725490196078431,0.752941176470588,
0.792156862745098);
#3152=COLOUR_RGB('Dark gray',0.250980392156863,0.282352941176471,0.32156862745098);
#3153=COLOUR_RGB('Stylus light gray',0.725490196078431,0.752941176470588,
0.792156862745098);
ENDSEC;
END-ISO-10303-21;
